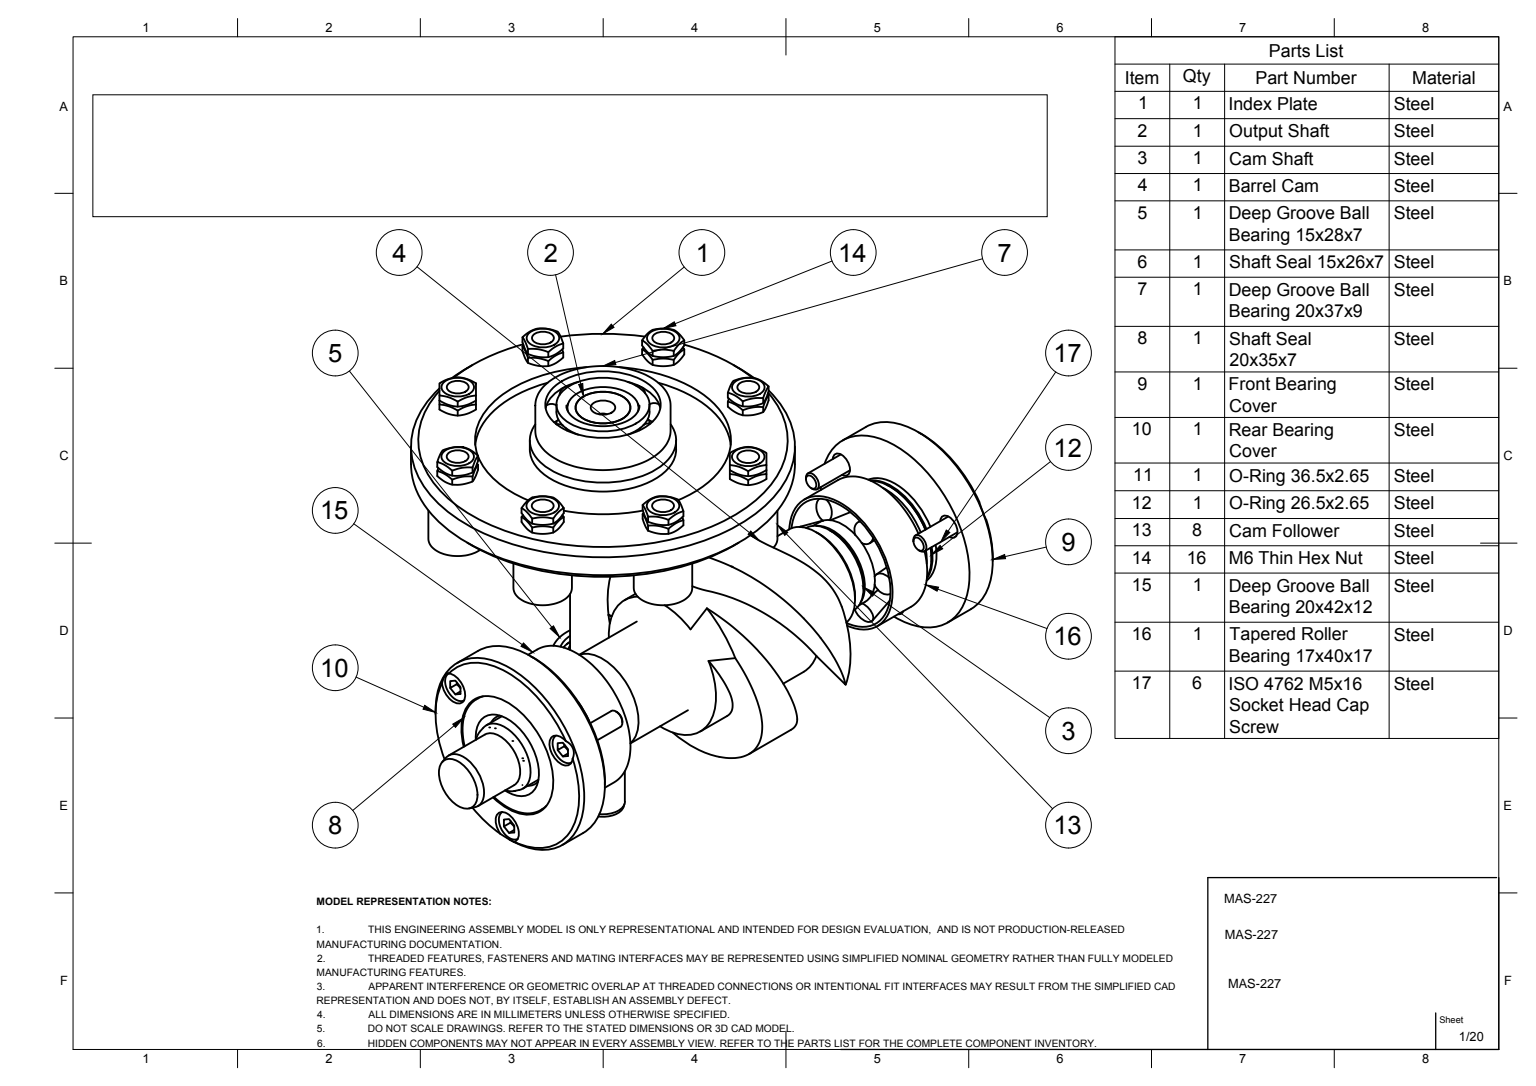
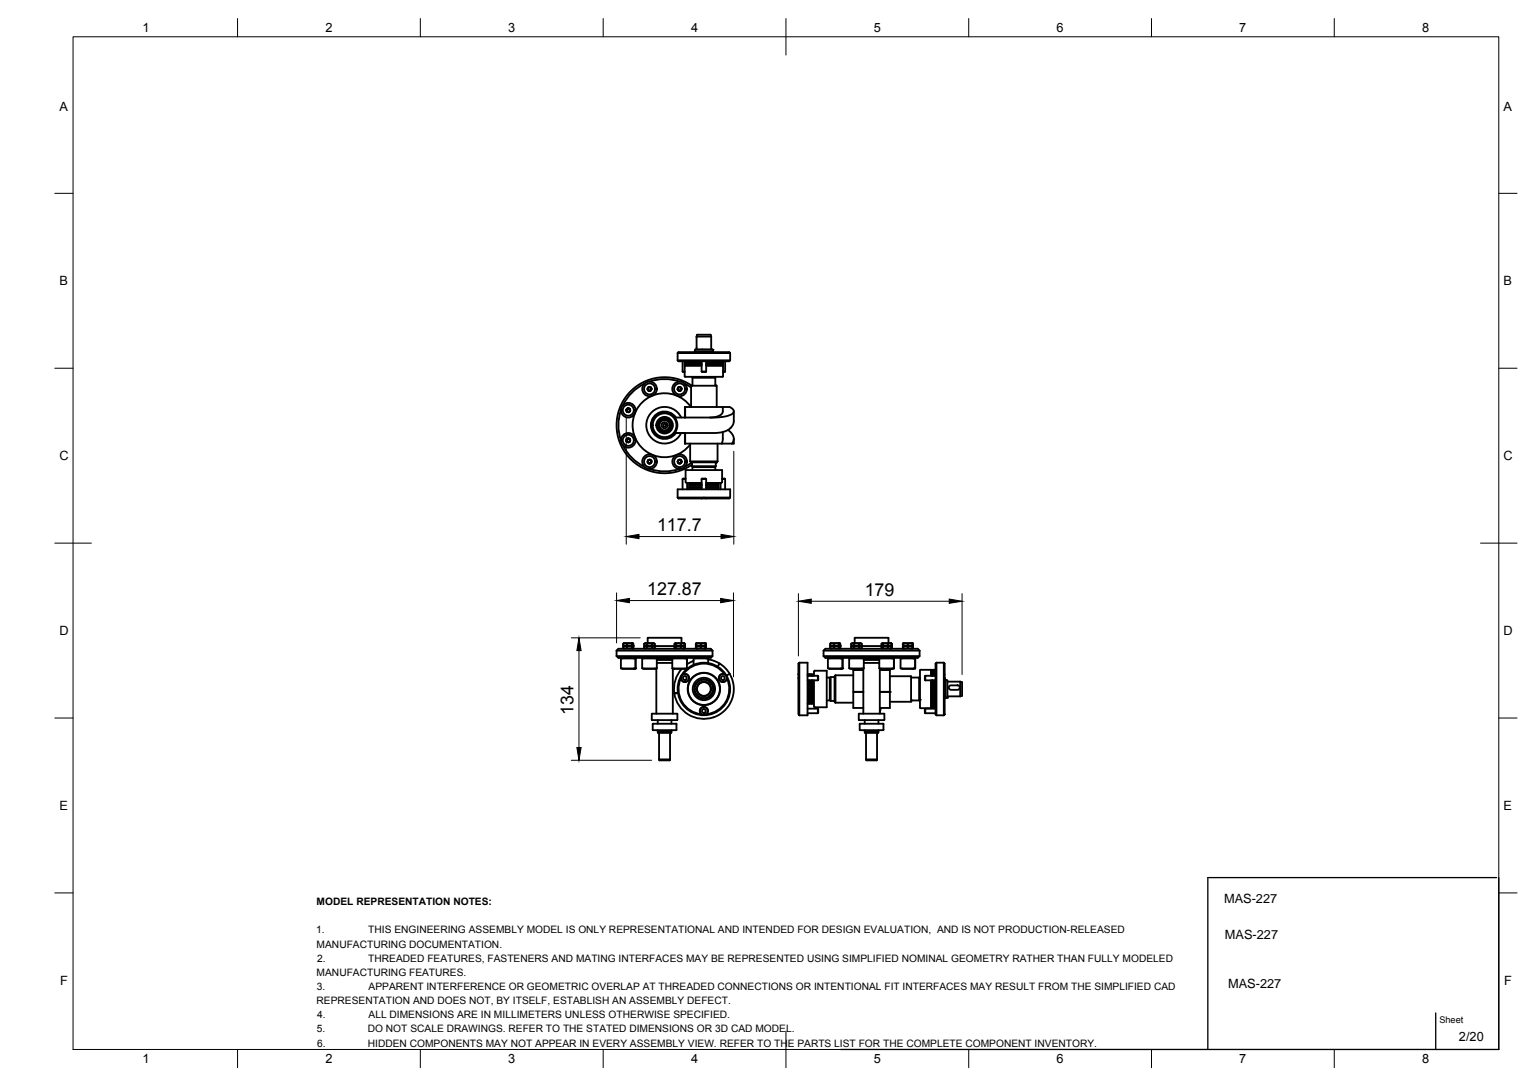
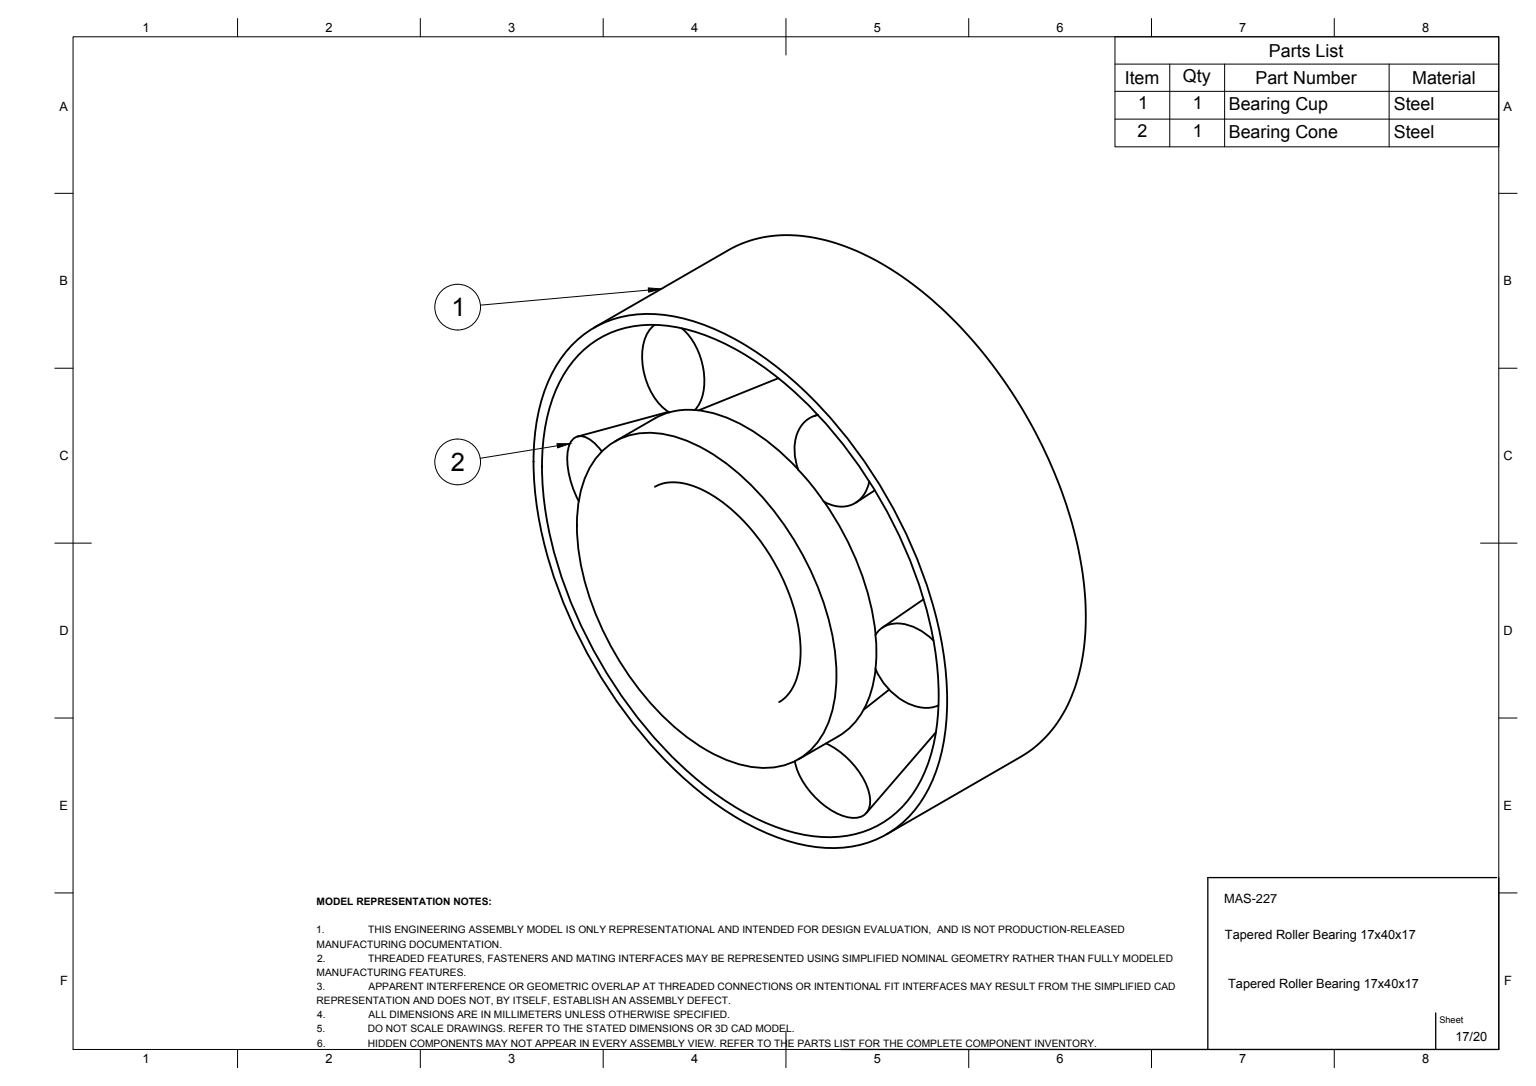
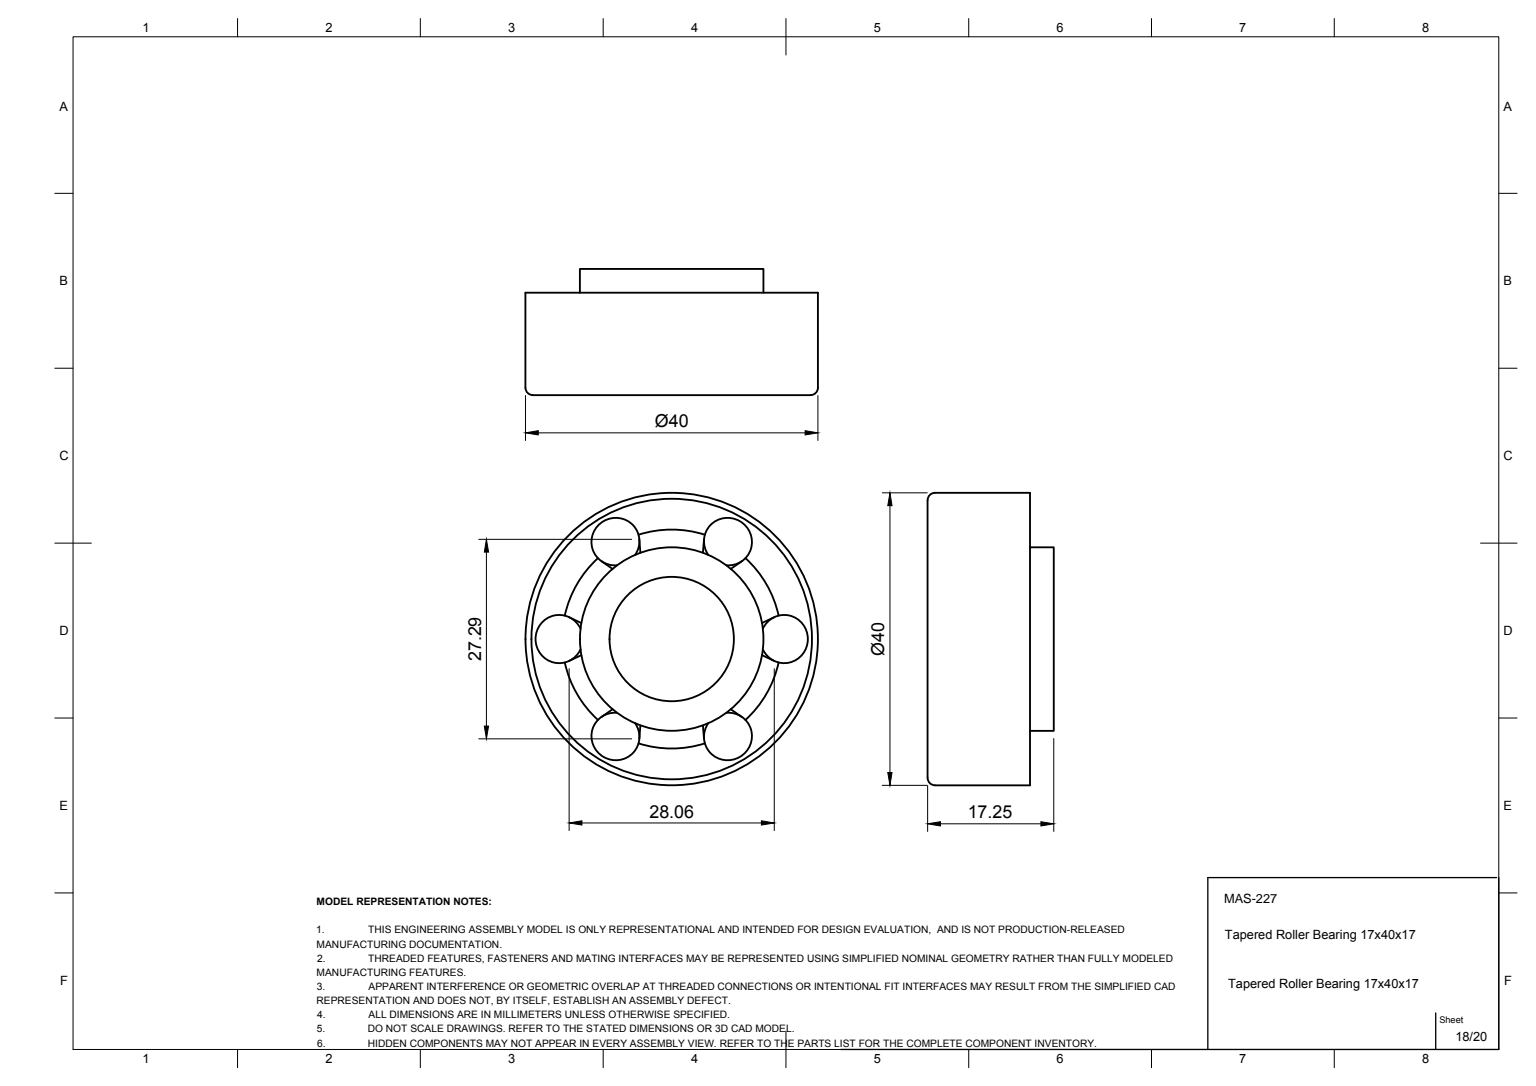
ISO-10303-21;
HEADER;
FILE_DESCRIPTION (('STEP AP214'),
    '1' );
FILE_NAME ( 'MAS-227', '2026-10-06T08:24:41', ( '' ), ( '' ), 'STEP AP214', 'Unspecified', '' );
FILE_SCHEMA (( 'AUTOMOTIVE_DESIGN' ));
ENDSEC;
DATA;
#1 = ORIENTED_EDGE ( 'NONE', *, *, #7056, .T. ) ;
#2 = LINE ( 'NONE', #16920, #12528 ) ;
#3 = CARTESIAN_POINT ( 'NONE',  ( -0.4535326485287288212, 0.08054850140359781641, 0.1903859677775356918 ) ) ;
#4 = EDGE_LOOP ( 'NONE', ( #17805, #23711 ) ) ;
#5 = EDGE_CURVE ( 'NONE', #3462, #12596, #11883, .T. ) ;
#6 = CARTESIAN_POINT ( 'NONE',  ( 0.3607825703614780388, 0.06309631803704385256, 0.08455817587619855746 ) ) ;
#7 = DIRECTION ( 'NONE',  ( -1.000000000000000000, 0.000000000000000000, 0.000000000000000000 ) ) ;
#8 = CARTESIAN_POINT ( 'NONE',  ( 0.4441657790107835790, 0.2564944395515610931, 1.766732283464566899 ) ) ;
#9 = CARTESIAN_POINT ( 'NONE',  ( -0.4441657790107816917, 0.2564944395515652564, 1.747047244094488194 ) ) ;
#10 = DIRECTION ( 'NONE',  ( 0.000000000000000000, 0.000000000000000000, -1.000000000000000000 ) ) ;
#11 = ORIENTED_EDGE ( 'NONE', *, *, #14941, .F. ) ;
#12 = ORIENTED_EDGE ( 'NONE', *, *, #1724, .F. ) ;
#13 = AXIS2_PLACEMENT_3D ( 'NONE', #19056, #4369, #12570 ) ;
#14 = CARTESIAN_POINT ( 'NONE',  ( 0.3392387706403788838, 0.1151913129404419922, -3.115157480314960647 ) ) ;
#15 = EDGE_LOOP ( 'NONE', ( #27467, #1263, #14618, #2315 ) ) ;
#16 = VECTOR ( 'NONE', #25665, 39.37007874015748143 ) ;
#17 = EDGE_LOOP ( 'NONE', ( #23357, #276 ) ) ;
#18 = FACE_OUTER_BOUND ( 'NONE', #11254, .T. ) ;
#19 = ( CONVERSION_BASED_UNIT ( 'INCH', #19315 ) LENGTH_UNIT ( ) NAMED_UNIT ( #4330 ) ) ;
#20 = CARTESIAN_POINT ( 'NONE',  ( 0.3339160553493882300, 0.9180073733179625606, -0.7185233507685039323 ) ) ;
#21 = CARTESIAN_POINT ( 'NONE',  ( 0.3324885138898234782, -0.04380447413659139394, 1.973425196850393970 ) ) ;
#22 = ORIENTED_EDGE ( 'NONE', *, *, #12287, .T. ) ;
#23 = EDGE_CURVE ( 'NONE', #19722, #14586, #4579, .T. ) ;
#24 = ORIENTED_EDGE ( 'NONE', *, *, #27873, .F. ) ;
#25 = VERTEX_POINT ( 'NONE', #21962 ) ;
#26 = AXIS2_PLACEMENT_3D ( 'NONE', #24045, #13033, #11185 ) ;
#27 = ORIENTED_EDGE ( 'NONE', *, *, #23684, .F. ) ;
#28 = EDGE_LOOP ( 'NONE', ( #27536, #25941, #6890, #26998 ) ) ;
#29 = ORIENTED_EDGE ( 'NONE', *, *, #17755, .F. ) ;
#30 = CARTESIAN_POINT ( 'NONE',  ( -0.5949363243629232079, -0.1357903337134990229, 0.2362204724409449064 ) ) ;
#31 = ( BOUNDED_CURVE ( )  B_SPLINE_CURVE ( 2, ( #4927, #4785, #24416 ),
 .UNSPECIFIED., .F., .T. ) 
 B_SPLINE_CURVE_WITH_KNOTS ( ( 3, 3 ),
 ( 0.000000000000000000, 0.5842180690389588982 ),
 .UNSPECIFIED. ) 
 CURVE ( )  GEOMETRIC_REPRESENTATION_ITEM ( )  RATIONAL_B_SPLINE_CURVE ( ( 1.000000000000000000, 1.154700538379253905, 1.000000000000000000 ) ) 
 REPRESENTATION_ITEM ( '' )  ) ;
#32 = ITEM_DEFINED_TRANSFORMATION ( 'NONE', 'NONE', #4428,  #11588 ) ;
#33 = EDGE_CURVE ( 'NONE', #1582, #19320, #13242, .T. ) ;
#34 = CARTESIAN_POINT ( 'NONE',  ( 0.3976891862754212137, 0.7181140751201200434, -0.6642661073933326943 ) ) ;
#35 = LINE ( 'NONE', #6897, #10289 ) ;
#36 = CARTESIAN_POINT ( 'NONE',  ( 0.4620608682196346573, 0.08206165078060492779, 0.1992125984251968684 ) ) ;
#37 = ORIENTED_EDGE ( 'NONE', *, *, #10875, .F. ) ;
#38 = AXIS2_PLACEMENT_3D ( 'NONE', #5001, #26071, #6729 ) ;
#39 = CARTESIAN_POINT ( 'NONE',  ( 0.000000000000000000, 0.000000000000000000, 0.06614173228346456601 ) ) ;
#40 = CARTESIAN_POINT ( 'NONE',  ( -2.184900367198595585E-17, 0.6212598425196850238, 0.2574827755769818483 ) ) ;
#41 = DIRECTION ( 'NONE',  ( 0.000000000000000000, 0.000000000000000000, -1.000000000000000000 ) ) ;
#42 = CARTESIAN_POINT ( 'NONE',  ( -0.3649820351482981340, -1.095990260593795451, -0.3743461065083169559 ) ) ;
#43 = CARTESIAN_POINT ( 'NONE',  ( 0.000000000000000000, 0.000000000000000000, 0.2362204724409449064 ) ) ;
#44 = DIRECTION ( 'NONE',  ( -0.000000000000000000, -1.000000000000000000, -0.000000000000000000 ) ) ;
#45 = EDGE_CURVE ( 'NONE', #18347, #8484, #23181, .T. ) ;
#46 = CARTESIAN_POINT ( 'NONE',  ( -0.08600259748440698682, 0.2165354330708661457, -3.223068998490977499 ) ) ;
#47 = ORIENTED_EDGE ( 'NONE', *, *, #24932, .T. ) ;
#48 = ORIENTED_EDGE ( 'NONE', *, *, #8188, .T. ) ;
#49 = DIRECTION ( 'NONE',  ( 0.000000000000000000, 0.000000000000000000, 1.000000000000000000 ) ) ;
#50 = AXIS2_PLACEMENT_3D ( 'NONE', #26604, #25051, #22376 ) ;
#51 = VERTEX_POINT ( 'NONE', #494 ) ;
#52 = VECTOR ( 'NONE', #14977, 39.37007874015748143 ) ;
#53 = DIRECTION ( 'NONE',  ( 0.000000000000000000, 0.000000000000000000, 1.000000000000000000 ) ) ;
#54 = DIRECTION ( 'NONE',  ( 1.000000000000000000, 0.000000000000000000, 0.000000000000000000 ) ) ;
#55 = EDGE_CURVE ( 'NONE', #27011, #13237, #9086, .T. ) ;
#56 = CARTESIAN_POINT ( 'NONE',  ( -0.5476281405333500718, 0.07214854559197644845, 0.9399606299212598381 ) ) ;
#57 = EDGE_CURVE ( 'NONE', #14897, #14790, #10537, .T. ) ;
#58 = CARTESIAN_POINT ( 'NONE',  ( 0.4771018889076559244, 0.3804760601893846794, 0.2362204724409449064 ) ) ;
#59 = ORIENTED_EDGE ( 'NONE', *, *, #13176, .F. ) ;
#60 = CARTESIAN_POINT ( 'NONE',  ( -0.4335958738490826581, -0.2505647196907692664, 0.09684793308443542803 ) ) ;
#61 = AXIS2_PLACEMENT_3D ( 'NONE', #22056, #14008, #15706 ) ;
#62 = CARTESIAN_POINT ( 'NONE',  ( 0.2428345617565153547, 0.2885915454824177218, 0.1992125984251968684 ) ) ;
#63 = ADVANCED_FACE ( 'NONE', ( #7520 ), #26320, .F. ) ;
#64 = CARTESIAN_POINT ( 'NONE',  ( 0.4157391792961063204, 0.3323952789219082882, 0.1322834645669291320 ) ) ;
#65 = CARTESIAN_POINT ( 'NONE',  ( 0.000000000000000000, 0.000000000000000000, -0.2618110236220472231 ) ) ;
#66 = DIRECTION ( 'NONE',  ( 0.000000000000000000, 0.000000000000000000, 1.000000000000000000 ) ) ;
#67 = CARTESIAN_POINT ( 'NONE',  ( 0.8031496062992127261, 0.000000000000000000, 0.4488188976377953110 ) ) ;
#68 = CARTESIAN_POINT ( 'NONE',  ( 0.1516263115863346334, -0.2937912646890007973, 0.3972688187320929099 ) ) ;
#69 = DIRECTION ( 'NONE',  ( 1.000000000000000000, 0.000000000000000000, 0.000000000000000000 ) ) ;
#70 = FACE_OUTER_BOUND ( 'NONE', #14571, .T. ) ;
#71 = DIRECTION ( 'NONE',  ( 0.000000000000000000, 0.000000000000000000, 1.000000000000000000 ) ) ;
#72 = CARTESIAN_POINT ( 'NONE',  ( 0.3339160553493882300, 0.7867001919223544082, -0.8344257386302499357 ) ) ;
#73 = AXIS2_PLACEMENT_3D ( 'NONE', #23725, #21593, #23590 ) ;
#74 = CARTESIAN_POINT ( 'NONE',  ( 0.1480156394741928561, -0.5526079293736928522, 0.9399606299212598381 ) ) ;
#75 = DIRECTION ( 'NONE',  ( -1.000000000000000000, 0.000000000000000000, 0.000000000000000000 ) ) ;
#76 = ORIENTED_EDGE ( 'NONE', *, *, #16694, .F. ) ;
#77 = CARTESIAN_POINT ( 'NONE',  ( 0.04673558830902516809, 0.3552036222399216903, -3.115157480314960647 ) ) ;
#78 = VECTOR ( 'NONE', #27167, 39.37007874015748854 ) ;
#79 = EDGE_LOOP ( 'NONE', ( #24549, #12991, #16155, #19629, #1630 ) ) ;
#80 = EDGE_LOOP ( 'NONE', ( #10881, #7158 ) ) ;
#81 = EDGE_CURVE ( 'NONE', #10766, #14002, #19559, .T. ) ;
#82 = CARTESIAN_POINT ( 'NONE',  ( 0.4856708409191422549, -0.1649135259639211148, -1.550196850393700920 ) ) ;
#83 = DIRECTION ( 'NONE',  ( 0.000000000000000000, 0.000000000000000000, 1.000000000000000000 ) ) ;
#84 = CARTESIAN_POINT ( 'NONE',  ( 0.5144793533649091311, -0.1379038425970198489, 1.747047244094488416 ) ) ;
#85 = ORIENTED_EDGE ( 'NONE', *, *, #20703, .F. ) ;
#86 = EDGE_CURVE ( 'NONE', #9806, #21006, #24069, .T. ) ;
#87 = FACE_BOUND ( 'NONE', #23508, .T. ) ;
#88 = VERTEX_POINT ( 'NONE', #13082 ) ;
#89 = DIRECTION ( 'NONE',  ( 0.000000000000000000, -1.000000000000000000, 0.000000000000000000 ) ) ;
#90 = CIRCLE ( 'NONE', #23529, 0.3937007874015748254 ) ;
#91 = CYLINDRICAL_SURFACE ( 'NONE', #13414, 0.4941010236220472751 ) ;
#92 = DIRECTION ( 'NONE',  ( -0.8660254037844387076, 0.4999999999999998890, 0.000000000000000000 ) ) ;
#93 = SURFACE_STYLE_USAGE ( .BOTH. , #2166 ) ;
#94 = DIRECTION ( 'NONE',  ( -1.000000000000000000, 0.000000000000000000, 0.000000000000000000 ) ) ;
#95 = CARTESIAN_POINT ( 'NONE',  ( 0.1709077104829875848, -0.4707213777573787672, 0.09684874903502814492 ) ) ;
#96 = ORIENTED_EDGE ( 'NONE', *, *, #21914, .F. ) ;
#97 = LINE ( 'NONE', #15591, #22935 ) ;
#98 = CARTESIAN_POINT ( 'NONE',  ( -0.4055118110236220486, 4.966087413865251393E-17, 0.3543307086614173040 ) ) ;
#99 = CARTESIAN_POINT ( 'NONE',  ( -0.3001918266901933974, 0.3912931228432126596, -1.550196850393700920 ) ) ;
#100 = PRODUCT_DEFINITION_CONTEXT ( 'detailed design', #9805, 'design' ) ;
#101 = CARTESIAN_POINT ( 'NONE',  ( 0.1458850421962362143, -0.4296318976989931815, -1.934055118110236338 ) ) ;
#102 = DIRECTION ( 'NONE',  ( -1.000000000000000000, 0.000000000000000000, 0.000000000000000000 ) ) ;
#103 = CARTESIAN_POINT ( 'NONE',  ( 0.1669771619554775988, -0.4570419016558947556, 0.1827409795206137999 ) ) ;
#104 = CARTESIAN_POINT ( 'NONE',  ( -0.6505662911506299162, -0.01797296504513622162, 0.07864818162991654704 ) ) ;
#105 = FILL_AREA_STYLE_COLOUR ( '', #1895 ) ;
#106 = DIRECTION ( 'NONE',  ( -1.000000000000000000, 0.000000000000000000, -0.000000000000000000 ) ) ;
#107 = ORIENTED_EDGE ( 'NONE', *, *, #20255, .T. ) ;
#108 = EDGE_LOOP ( 'NONE', ( #16831, #22102, #23011, #14973, #23434 ) ) ;
#109 = ADVANCED_FACE ( 'NONE', ( #134 ), #14626, .F. ) ;
#110 = CIRCLE ( 'NONE', #17215, 0.4848217985909654137 ) ;
#111 = FACE_OUTER_BOUND ( 'NONE', #23572, .T. ) ;
#112 = AXIS2_PLACEMENT_3D ( 'NONE', #26701, #7362, #3107 ) ;
#113 = CARTESIAN_POINT ( 'NONE',  ( -0.3350125228558759050, 0.2937477835494528011, -1.934055118110236560 ) ) ;
#114 = EDGE_CURVE ( 'NONE', #14474, #3555, #20012, .T. ) ;
#115 = CARTESIAN_POINT ( 'NONE',  ( -0.7432982829791772161, 0.2032415433700952845, -0.2614846436432287091 ) ) ;
#116 = EDGE_LOOP ( 'NONE', ( #3270, #475, #22588, #2347 ) ) ;
#117 = DIRECTION ( 'NONE',  ( -1.000000000000000000, 0.000000000000000000, 0.000000000000000000 ) ) ;
#118 = CARTESIAN_POINT ( 'NONE',  ( -0.1839420097223181394, -0.5417097841048805762, 0.9399606299212598381 ) ) ;
#119 = CARTESIAN_POINT ( 'NONE',  ( 0.3334645669291338987, -0.9593003268715946108, -0.8847456892490688229 ) ) ;
#120 = ( REPRESENTATION_RELATIONSHIP ('NONE','NONE', #12434, #25798 ) REPRESENTATION_RELATIONSHIP_WITH_TRANSFORMATION ( #8739 )SHAPE_REPRESENTATION_RELATIONSHIP( ) ) ;
#121 = DIRECTION ( 'NONE',  ( 0.000000000000000000, -0.8660254037844385966, 0.4999999999999998335 ) ) ;
#122 = AXIS2_PLACEMENT_3D ( 'NONE', #22797, #14633, #3420 ) ;
#123 = CARTESIAN_POINT ( 'NONE',  ( 0.3858827008519146728, -0.2227458012931471110, -1.934055118110236338 ) ) ;
#124 = CARTESIAN_POINT ( 'NONE',  ( 0.3233561589689052385, -0.1867299569291582528, -3.115157480314960647 ) ) ;
#125 = DIRECTION ( 'NONE',  ( 0.000000000000000000, -1.000000000000000000, 0.000000000000000000 ) ) ;
#126 = CARTESIAN_POINT ( 'NONE',  ( 0.0005789221761808661720, 0.4692909815006409691, 0.1992125984251968684 ) ) ;
#127 = DIRECTION ( 'NONE',  ( -1.000000000000000000, 0.000000000000000000, 0.000000000000000000 ) ) ;
#128 = CARTESIAN_POINT ( 'NONE',  ( 0.000000000000000000, 0.000000000000000000, 0.01181102362204724393 ) ) ;
#129 = EDGE_CURVE ( 'NONE', #7282, #11900, #2406, .T. ) ;
#130 = TOROIDAL_SURFACE ( 'NONE', #25799, 0.5610236220472440971, 0.1003937007874015908 ) ;
#131 = DIRECTION ( 'NONE',  ( 0.000000000000000000, 0.000000000000000000, -1.000000000000000000 ) ) ;
#132 = CIRCLE ( 'NONE', #21747, 0.6299212598425196763 ) ;
#133 = ORIENTED_EDGE ( 'NONE', *, *, #949, .F. ) ;
#134 = FACE_OUTER_BOUND ( 'NONE', #7605, .T. ) ;
#135 = ORIENTED_EDGE ( 'NONE', *, *, #15589, .F. ) ;
#136 = CARTESIAN_POINT ( 'NONE',  ( 0.000000000000000000, 0.000000000000000000, 0.2362204724409449064 ) ) ;
#137 = DIRECTION ( 'NONE',  ( 0.000000000000000000, 0.000000000000000000, 1.000000000000000000 ) ) ;
#138 = CARTESIAN_POINT ( 'NONE',  ( -0.4069448477556107946, -0.3121994997598286914, 1.766732283464566899 ) ) ;
#139 = DIRECTION ( 'NONE',  ( 0.000000000000000000, 0.000000000000000000, 1.000000000000000000 ) ) ;
#140 = ORIENTED_EDGE ( 'NONE', *, *, #5854, .T. ) ;
#141 = TOROIDAL_SURFACE ( 'NONE', #14548, 0.5915354330708662012, 0.05216535433070866590 ) ;
#142 = ORIENTED_EDGE ( 'NONE', *, *, #15280, .T. ) ;
#144 = CARTESIAN_POINT ( 'NONE',  ( 0.3460635936745020680, -0.09269288654273737105, -3.115157480314960647 ) ) ;
#143 = CARTESIAN_POINT ( 'NONE',  ( 0.5614173959481695286, 0.4467232815848914962, 0.1601585119481469810 ) ) ;
#145 = ORIENTED_EDGE ( 'NONE', *, *, #17289, .F. ) ;
#146 = CARTESIAN_POINT ( 'NONE',  ( -2.183966630091013010E-17, 0.6212598425196852459, 0.09684793308443542803 ) ) ;
#147 = VERTEX_POINT ( 'NONE', #612 ) ;
#148 = CARTESIAN_POINT ( 'NONE',  ( 0.07874015748031495954, -0.04546065111729338803, -0.4724409448818898127 ) ) ;
#149 = DIRECTION ( 'NONE',  ( 1.000000000000000000, 0.000000000000000000, 0.000000000000000000 ) ) ;
#150 = ADVANCED_FACE ( 'NONE', ( #5405 ), #14023, .T. ) ;
#151 = ORIENTED_EDGE ( 'NONE', *, *, #4349, .F. ) ;
#152 = VERTEX_POINT ( 'NONE', #7235 ) ;
#153 = AXIS2_PLACEMENT_3D ( 'NONE', #12101, #3470, #22847 ) ;
#154 = ADVANCED_FACE ( 'NONE', ( #2979 ), #26440, .T. ) ;
#155 = CARTESIAN_POINT ( 'NONE',  ( 0.000000000000000000, 0.000000000000000000, 0.9055118110027171596 ) ) ;
#156 = ORIENTED_EDGE ( 'NONE', *, *, #27125, .T. ) ;
#157 = ORIENTED_EDGE ( 'NONE', *, *, #9364, .T. ) ;
#158 = VERTEX_POINT ( 'NONE', #15724 ) ;
#159 = CARTESIAN_POINT ( 'NONE',  ( -0.1771653543307086520, -5.663984251968503442E-18, 0.000000000000000000 ) ) ;
#160 = DIRECTION ( 'NONE',  ( 0.000000000000000000, 0.000000000000000000, 1.000000000000000000 ) ) ;
#161 = CARTESIAN_POINT ( 'NONE',  ( 0.000000000000000000, 0.000000000000000000, -0.1033464566929133965 ) ) ;
#162 = CARTESIAN_POINT ( 'NONE',  ( 0.09842519685039370636, 0.2165354330708661457, -3.456364829396325167 ) ) ;
#163 = PRODUCT ( 'M6 Thin Hex Nut', 'M6 Thin Hex Nut', '', ( #11511 ) ) ;
#164 = CIRCLE ( 'NONE', #26696, 1.988188976448617584 ) ;
#165 = CARTESIAN_POINT ( 'NONE',  ( 0.000000000000000000, 0.000000000000000000, -3.278217716535432842E-17 ) ) ;
#166 = CARTESIAN_POINT ( 'NONE',  ( 0.1490609433494345659, -0.2352065284464384953, -0.4168512521180542385 ) ) ;
#167 = DIRECTION ( 'NONE',  ( 1.000000000000000000, 0.000000000000000000, 0.000000000000000000 ) ) ;
#168 = CARTESIAN_POINT ( 'NONE',  ( -0.2120693917185543231, -0.5839438448129543602, 0.09684874924366436433 ) ) ;
#169 = EDGE_CURVE ( 'NONE', #21708, #16172, #21378, .T. ) ;
#170 = CIRCLE ( 'NONE', #27197, 0.2952755905264887182 ) ;
#171 = CARTESIAN_POINT ( 'NONE',  ( -0.3799403784234969272, -1.031940123604548010, -0.2795979895621366063 ) ) ;
#172 = CARTESIAN_POINT ( 'NONE',  ( -0.6029881478123397809, 1.118968434182175953, 0.03326447829408156476 ) ) ;
#173 = FACE_OUTER_BOUND ( 'NONE', #11804, .T. ) ;
#174 = CARTESIAN_POINT ( 'NONE',  ( -0.07870736599817811097, 0.1968503937007873850, -3.212150913008701814 ) ) ;
#175 = EDGE_LOOP ( 'NONE', ( #22367, #5338, #24383, #19393 ) ) ;
#176 = ADVANCED_FACE ( 'NONE', ( #13590 ), #15218, .F. ) ;
#177 = DIRECTION ( 'NONE',  ( 0.000000000000000000, 0.000000000000000000, 1.000000000000000000 ) ) ;
#178 = CARTESIAN_POINT ( 'NONE',  ( 0.000000000000000000, 0.000000000000000000, 0.2362204724409449064 ) ) ;
#179 = VECTOR ( 'NONE', #19878, 39.37007874015748143 ) ;
#180 = ORIENTED_EDGE ( 'NONE', *, *, #22193, .F. ) ;
#181 = ( BOUNDED_CURVE ( )  B_SPLINE_CURVE ( 3, ( #15130, #19634, #17231, #21476 ),
 .UNSPECIFIED., .F., .F. ) 
 B_SPLINE_CURVE_WITH_KNOTS ( ( 4, 4 ),
 ( 6.170019055269735375, 6.396351559089437089 ),
 .UNSPECIFIED. ) 
 CURVE ( )  GEOMETRIC_REPRESENTATION_ITEM ( )  RATIONAL_B_SPLINE_CURVE ( ( 1.000000000000000000, 0.9957356870045847019, 0.9957356870045847019, 1.000000000000000000 ) ) 
 REPRESENTATION_ITEM ( '' )  ) ;
#182 = CIRCLE ( 'NONE', #19069, 0.2952755905511810774 ) ;
#183 = CARTESIAN_POINT ( 'NONE',  ( 0.1259842519685039353, 0.1751968503937007815, 0.000000000000000000 ) ) ;
#184 = CARTESIAN_POINT ( 'NONE',  ( 0.4932478747986535628, 0.08657132889677619791, 0.09684874903502814492 ) ) ;
#185 = CARTESIAN_POINT ( 'NONE',  ( 0.0007595033562148819414, 0.6881885572739390167, 0.1322834645669291320 ) ) ;
#186 = B_SPLINE_CURVE_WITH_KNOTS ( 'NONE', 3,
 ( #3405, #6229, #8475, #4376, #23337, #25576 ),
 .UNSPECIFIED., .F., .F.,
 ( 4, 2, 4 ),
 ( 0.2291966065698869959, 0.2305109203526899964, 0.2318252341354939960 ),
 .UNSPECIFIED. ) ;
#187 = ORIENTED_EDGE ( 'NONE', *, *, #16548, .F. ) ;
#188 = CARTESIAN_POINT ( 'NONE',  ( -0.4382482975805212511, 0.3362148458989001609, 0.9399606299212598381 ) ) ;
#189 = ORIENTED_EDGE ( 'NONE', *, *, #329, .F. ) ;
#190 = CARTESIAN_POINT ( 'NONE',  ( -0.6299212598425196763, -0.4724409448818898127, -0.8182917201112815953 ) ) ;
#191 = ORIENTED_EDGE ( 'NONE', *, *, #12482, .T. ) ;
#192 = DIRECTION ( 'NONE',  ( -1.000000000000000000, 0.000000000000000000, 0.000000000000000000 ) ) ;
#193 = CIRCLE ( 'NONE', #14146, 0.1181102362204720091 ) ;
#194 = CARTESIAN_POINT ( 'NONE',  ( 0.000000000000000000, 0.000000000000000000, -0.2204724409448818867 ) ) ;
#195 = CARTESIAN_POINT ( 'NONE',  ( 0.000000000000000000, 0.000000000000000000, -3.278217716535432842E-17 ) ) ;
#196 = CARTESIAN_POINT ( 'NONE',  ( -0.6751968503937006982, 0.000000000000000000, -0.2618110236220472231 ) ) ;
#197 = CARTESIAN_POINT ( 'NONE',  ( -0.3149606299212598381, 0.000000000000000000, -0.03543307086614204404 ) ) ;
#198 = CARTESIAN_POINT ( 'NONE',  ( -0.1709077104829878069, -0.4707213777573787672, 0.09684874903502814492 ) ) ;
#199 = CARTESIAN_POINT ( 'NONE',  ( -0.3665264996331779601, -0.2116141732283464416, 0.1377952755905511861 ) ) ;
#200 = DIRECTION ( 'NONE',  ( 0.000000000000000000, -1.000000000000000000, 0.000000000000000000 ) ) ;
#201 = DIRECTION ( 'NONE',  ( -0.000000000000000000, -1.000000000000000000, -0.000000000000000000 ) ) ;
#202 = DIRECTION ( 'NONE',  ( 0.000000000000000000, 0.000000000000000000, 1.000000000000000000 ) ) ;
#203 = ADVANCED_FACE ( 'NONE', ( #17324 ), #15936, .F. ) ;
#204 = CIRCLE ( 'NONE', #17722, 0.6212598425196850238 ) ;
#205 = CARTESIAN_POINT ( 'NONE',  ( 0.07472527936312040042, -0.5671862884095228985, 0.9399606299212598381 ) ) ;
#206 = DIRECTION ( 'NONE',  ( 0.000000000000000000, 1.000000000000000000, 0.000000000000000000 ) ) ;
#207 = ORIENTED_EDGE ( 'NONE', *, *, #6942, .F. ) ;
#208 = CARTESIAN_POINT ( 'NONE',  ( -0.01968503937007897581, -0.8214970631411201429, 0.000000000000000000 ) ) ;
#209 = EDGE_CURVE ( 'NONE', #16657, #13154, #17294, .T. ) ;
#210 = CIRCLE ( 'NONE', #27230, 0.6212598425196850238 ) ;
#211 = EDGE_CURVE ( 'NONE', #8069, #8578, #17150, .T. ) ;
#212 = AXIS2_PLACEMENT_3D ( 'NONE', #21327, #27824, #8463 ) ;
#213 = ORIENTED_EDGE ( 'NONE', *, *, #16639, .F. ) ;
#214 = VERTEX_POINT ( 'NONE', #20374 ) ;
#215 = CARTESIAN_POINT ( 'NONE',  ( 0.4954757973265890847, -0.2860025288253325582, 0.9399606299212601712 ) ) ;
#216 = LINE ( 'NONE', #2154, #15629 ) ;
#217 = CARTESIAN_POINT ( 'NONE',  ( -1.928513779527558736E-17, 0.000000000000000000, -0.4566929133858267376 ) ) ;
#218 = VERTEX_POINT ( 'NONE', #1034 ) ;
#219 = VECTOR ( 'NONE', #3397, 39.37007874015748143 ) ;
#220 = CARTESIAN_POINT ( 'NONE',  ( 0.000000000000000000, 0.000000000000000000, 0.1771653543307086520 ) ) ;
#221 = EDGE_LOOP ( 'NONE', ( #12338, #6881, #25054, #27642 ) ) ;
#222 = SURFACE_STYLE_USAGE ( .BOTH. , #19537 ) ;
#223 = CARTESIAN_POINT ( 'NONE',  ( 0.0005057506112066243896, 0.6881888373222778688, 0.3401591245381555551 ) ) ;
#224 = ( CONVERSION_BASED_UNIT ( 'INCH', #8931 ) LENGTH_UNIT ( ) NAMED_UNIT ( #18982 ) ) ;
#225 = CIRCLE ( 'NONE', #16892, 0.5007874015748031704 ) ;
#226 = CARTESIAN_POINT ( 'NONE',  ( 0.0005189969344232283309, 0.3771649972486724733, 0.07637795275590551769 ) ) ;
#227 = AXIS2_PLACEMENT_3D ( 'NONE', #3508, #14722, #27552 ) ;
#228 = ORIENTED_EDGE ( 'NONE', *, *, #21922, .T. ) ;
#229 = CARTESIAN_POINT ( 'NONE',  ( 0.03008364706454716778, 0.1136516277932332619, 0.1968503937007874127 ) ) ;
#230 = ADVANCED_FACE ( 'NONE', ( #18229 ), #8731, .T. ) ;
#231 = DIRECTION ( 'NONE',  ( 0.000000000000000000, 0.000000000000000000, 1.000000000000000000 ) ) ;
#232 = EDGE_CURVE ( 'NONE', #4548, #1758, #3760, .T. ) ;
#233 = EDGE_CURVE ( 'NONE', #14152, #23049, #22735, .T. ) ;
#234 = AXIS2_PLACEMENT_3D ( 'NONE', #13814, #26508, #13665 ) ;
#235 = EDGE_CURVE ( 'NONE', #27620, #935, #8316, .T. ) ;
#236 = CARTESIAN_POINT ( 'NONE',  ( -0.6370261810203012853, -0.04389326872400071272, -0.2373533611760622331 ) ) ;
#237 = FACE_OUTER_BOUND ( 'NONE', #646, .T. ) ;
#238 = SURFACE_STYLE_USAGE ( .BOTH. , #19827 ) ;
#239 = EDGE_LOOP ( 'NONE', ( #22677, #15160 ) ) ;
#240 = VERTEX_POINT ( 'NONE', #18659 ) ;
#241 = EDGE_CURVE ( 'NONE', #21409, #11103, #22772, .T. ) ;
#242 = AXIS2_PLACEMENT_3D ( 'NONE', #867, #7637, #22743 ) ;
#243 = FACE_OUTER_BOUND ( 'NONE', #27157, .T. ) ;
#244 = CIRCLE ( 'NONE', #20043, 0.1751968503937007815 ) ;
#245 = DIRECTION ( 'NONE',  ( -1.000000000000000000, 0.000000000000000000, 0.000000000000000000 ) ) ;
#246 = CARTESIAN_POINT ( 'NONE',  ( 0.1490609433615242285, 0.4786070381542913421, 0.000000000000000000 ) ) ;
#247 = VERTEX_POINT ( 'NONE', #23212 ) ;
#248 = CARTESIAN_POINT ( 'NONE',  ( 0.3998447049182889956, 0.4754871227240441423, 0.2574803149606298969 ) ) ;
#249 = ORIENTED_EDGE ( 'NONE', *, *, #1427, .F. ) ;
#250 = CARTESIAN_POINT ( 'NONE',  ( -0.7795729917428700917, 0.3988254141273629982, 0.006455232907575630084 ) ) ;
#251 = EDGE_CURVE ( 'NONE', #10904, #1560, #4337, .T. ) ;
#252 = ORIENTED_EDGE ( 'NONE', *, *, #21026, .F. ) ;
#253 = DIRECTION ( 'NONE',  ( -1.000000000000000000, 0.000000000000000000, 0.000000000000000000 ) ) ;
#254 = CARTESIAN_POINT ( 'NONE',  ( 0.3722026523000413478, 4.558167867734008572E-17, -0.07578740157480315376 ) ) ;
#255 = CARTESIAN_POINT ( 'NONE',  ( -0.03736310157557653361, -0.5708661417322835607, 0.9399606299212598381 ) ) ;
#256 = DIRECTION ( 'NONE',  ( 0.000000000000000000, 0.000000000000000000, 1.000000000000000000 ) ) ;
#257 = AXIS2_PLACEMENT_3D ( 'NONE', #24962, #7448, #3195 ) ;
#258 = CARTESIAN_POINT ( 'NONE',  ( 0.4303681241740789920, -0.1153557615287144622, -1.934055118110236338 ) ) ;
#259 = CARTESIAN_POINT ( 'NONE',  ( -0.3233561589689049609, -0.1867299569291588357, -3.115157480314960647 ) ) ;
#260 = DIRECTION ( 'NONE',  ( 0.000000000000000000, -0.4702444477782212195, 0.8825362085114445421 ) ) ;
#261 = CARTESIAN_POINT ( 'NONE',  ( 0.2965233727166233790, 0.3524965443697388734, 0.1771653543307087630 ) ) ;
#262 = DIRECTION ( 'NONE',  ( 0.8660254037844385966, 0.4999999999999998335, 0.000000000000000000 ) ) ;
#263 = ORIENTED_EDGE ( 'NONE', *, *, #3631, .F. ) ;
#264 = DIRECTION ( 'NONE',  ( -0.000000000000000000, -1.000000000000000000, -0.000000000000000000 ) ) ;
#265 = CIRCLE ( 'NONE', #4300, 0.01377952755905510404 ) ;
#266 = CIRCLE ( 'NONE', #11488, 0.4692913385826771866 ) ;
#267 = EDGE_CURVE ( 'NONE', #4877, #9806, #20517, .T. ) ;
#268 = ORIENTED_EDGE ( 'NONE', *, *, #11086, .F. ) ;
#269 = CARTESIAN_POINT ( 'NONE',  ( 0.3751294191746885609, 0.2999672986753447734, 0.2362204724409446843 ) ) ;
#270 = APPLICATION_PROTOCOL_DEFINITION ( 'draft international standard', 'automotive_design', 1998, #14720 ) ;
#271 = CARTESIAN_POINT ( 'NONE',  ( 0.5118110236220472231, 0.03349795313260757468, 1.766732283464566899 ) ) ;
#272 = EDGE_CURVE ( 'NONE', #27250, #26868, #24521, .T. ) ;
#273 = AXIS2_PLACEMENT_3D ( 'NONE', #1316, #18082, #27170 ) ;
#274 = ORIENTED_EDGE ( 'NONE', *, *, #6413, .T. ) ;
#275 = ORIENTED_EDGE ( 'NONE', *, *, #12081, .F. ) ;
#276 = ORIENTED_EDGE ( 'NONE', *, *, #1809, .T. ) ;
#277 = CARTESIAN_POINT ( 'NONE',  ( 0.2362439534887500470, 0.2693339498142248156, -3.115157480314960647 ) ) ;
#279 = DIRECTION ( 'NONE',  ( 0.000000000000000000, 1.000000000000000000, 0.000000000000000000 ) ) ;
#278 = ( REPRESENTATION_RELATIONSHIP ('NONE','NONE', #12434, #6338 ) REPRESENTATION_RELATIONSHIP_WITH_TRANSFORMATION ( #9729 )SHAPE_REPRESENTATION_RELATIONSHIP( ) ) ;
#280 = VERTEX_POINT ( 'NONE', #5695 ) ;
#281 = FACE_OUTER_BOUND ( 'NONE', #3824, .T. ) ;
#282 = DIRECTION ( 'NONE',  ( -5.737213000000000442E-16, 1.000000000000000000, -1.224646799147353207E-16 ) ) ;
#283 = CARTESIAN_POINT ( 'NONE',  ( 0.2521176338356670432, 0.2211428102655656758, 1.953740157480315043 ) ) ;
#284 = EDGE_CURVE ( 'NONE', #11054, #21365, #5605, .T. ) ;
#285 = VERTEX_POINT ( 'NONE', #25460 ) ;
#286 = B_SPLINE_CURVE_WITH_KNOTS ( 'NONE', 3,
 ( #23808, #10659, #8682, #25644, #1905, #25921 ),
 .UNSPECIFIED., .F., .F.,
 ( 4, 2, 4 ),
 ( 0.7157687286427140139, 0.7172350147555670574, 0.7187013008684199900 ),
 .UNSPECIFIED. ) ;
#287 = LINE ( 'NONE', #8993, #4640 ) ;
#288 = VECTOR ( 'NONE', #25733, 39.37007874015748143 ) ;
#289 = ORIENTED_EDGE ( 'NONE', *, *, #13370, .F. ) ;
#290 = VERTEX_POINT ( 'NONE', #22923 ) ;
#291 = ORIENTED_EDGE ( 'NONE', *, *, #20836, .F. ) ;
#292 = DIRECTION ( 'NONE',  ( -1.000000000000000000, -7.017815999999999636E-18, 0.000000000000000000 ) ) ;
#293 = CARTESIAN_POINT ( 'NONE',  ( 0.6947676139410623453, 0.7729092381583980709, -0.02125091332446964881 ) ) ;
#294 = ORIENTED_EDGE ( 'NONE', *, *, #2324, .F. ) ;
#295 = VECTOR ( 'NONE', #17634, 39.37007874015748143 ) ;
#296 = EDGE_CURVE ( 'NONE', #10766, #14592, #15963, .T. ) ;
#297 = CARTESIAN_POINT ( 'NONE',  ( -0.6708219662590964028, -0.1536294932067021612, 0.1322818203437344520 ) ) ;
#298 = EDGE_CURVE ( 'NONE', #7459, #10848, #1546, .T. ) ;
#299 = CARTESIAN_POINT ( 'NONE',  ( -0.5190862322091315262, -0.1177929122753175184, 0.3401574803149606252 ) ) ;
#300 = ADVANCED_FACE ( 'NONE', ( #3258 ), #20928, .T. ) ;
#301 = ORIENTED_EDGE ( 'NONE', *, *, #18506, .T. ) ;
#302 = AXIS2_PLACEMENT_3D ( 'NONE', #2958, #11178, #15703 ) ;
#303 = DIRECTION ( 'NONE',  ( 0.000000000000000000, 0.000000000000000000, -1.000000000000000000 ) ) ;
#304 = B_SPLINE_CURVE_WITH_KNOTS ( 'NONE', 3,
 ( #11360, #4990, #21548, #4455 ),
 .UNSPECIFIED., .F., .F.,
 ( 4, 4 ),
 ( 1.743059029969425078, 1.744705333033724992 ),
 .UNSPECIFIED. ) ;
#305 = VECTOR ( 'NONE', #25355, 39.37007874015748854 ) ;
#306 = CARTESIAN_POINT ( 'NONE',  ( 0.07870736599818350943, 0.1968503937007873850, -3.212150913008773312 ) ) ;
#307 = ORIENTED_EDGE ( 'NONE', *, *, #13471, .F. ) ;
#308 = DIRECTION ( 'NONE',  ( 0.7660444431189782355, 0.6427876096865391409, 0.000000000000000000 ) ) ;
#309 = ( CONVERSION_BASED_UNIT ( 'INCH', #689 ) LENGTH_UNIT ( ) NAMED_UNIT ( #9238 ) ) ;
#310 = CARTESIAN_POINT ( 'NONE',  ( 0.3362554559023149814, -0.1141145734059788724, 1.953740157480315043 ) ) ;
#311 = ORIENTED_EDGE ( 'NONE', *, *, #16319, .F. ) ;
#312 = DIRECTION ( 'NONE',  ( 0.000000000000000000, 0.000000000000000000, 1.000000000000000000 ) ) ;
#313 = DIRECTION ( 'NONE',  ( -1.000000000000000000, 0.000000000000000000, 0.000000000000000000 ) ) ;
#314 = PLANE ( 'NONE',  #8850 ) ;
#315 = FACE_OUTER_BOUND ( 'NONE', #4485, .T. ) ;
#316 = ORIENTED_EDGE ( 'NONE', *, *, #13974, .F. ) ;
#317 = CARTESIAN_POINT ( 'NONE',  ( 0.4783323773986625782, 0.2762247810518427271, 0.9399606299212598381 ) ) ;
#318 = ORIENTED_EDGE ( 'NONE', *, *, #26206, .F. ) ;
#319 = DIRECTION ( 'NONE',  ( 1.000000000000000000, 0.000000000000000000, 0.000000000000000000 ) ) ;
#320 = ORIENTED_EDGE ( 'NONE', *, *, #13672, .F. ) ;
#321 = VECTOR ( 'NONE', #12149, 39.37007874015748143 ) ;
#322 = FACE_OUTER_BOUND ( 'NONE', #12534, .T. ) ;
#323 = CARTESIAN_POINT ( 'NONE',  ( -0.4126915023524561632, -0.2375990495015092296, 0.2330651858026694390 ) ) ;
#324 = AXIS2_PLACEMENT_3D ( 'NONE', #9492, #22508, #24756 ) ;
#325 = CARTESIAN_POINT ( 'NONE',  ( -0.1716509673353403542, -0.4704508543867079173, 0.09684874903502814492 ) ) ;
#326 = CARTESIAN_POINT ( 'NONE',  ( -0.1196556571310431333, -0.3272932875252256291, 0.1166443193928402983 ) ) ;
#327 = CARTESIAN_POINT ( 'NONE',  ( 0.5692936381926190226, -0.3294684677443725507, 0.2081850588275903358 ) ) ;
#328 = FACE_OUTER_BOUND ( 'NONE', #1258, .T. ) ;
#329 = EDGE_CURVE ( 'NONE', #8378, #18994, #15536, .T. ) ;
#330 = ORIENTED_EDGE ( 'NONE', *, *, #18348, .T. ) ;
#331 = CARTESIAN_POINT ( 'NONE',  ( 0.000000000000000000, 0.000000000000000000, -0.2342519685039370358 ) ) ;
#332 = CARTESIAN_POINT ( 'NONE',  ( -0.2529800193559212929, 0.5131133041954029084, 0.9399606299212598381 ) ) ;
#333 = VERTEX_POINT ( 'NONE', #9774 ) ;
#334 = CARTESIAN_POINT ( 'NONE',  ( -0.5118110236220472231, 0.000000000000000000, 1.953740157480315043 ) ) ;
#335 = CARTESIAN_POINT ( 'NONE',  ( 0.000000000000000000, 0.000000000000000000, 0.2362204724409449064 ) ) ;
#336 = AXIS2_PLACEMENT_3D ( 'NONE', #6221, #5940, #1966 ) ;
#337 = CONICAL_SURFACE ( 'NONE', #25107, 0.06200787401574805319, 1.029744258088332254 ) ;
#338 = ORIENTED_EDGE ( 'NONE', *, *, #23140, .F. ) ;
#339 = VERTEX_POINT ( 'NONE', #12317 ) ;
#340 = CIRCLE ( 'NONE', #27828, 0.1181102362204724532 ) ;
#341 = B_SPLINE_CURVE_WITH_KNOTS ( 'NONE', 3,
 ( #20281, #13782, #13925, #26772, #18280, #24375, #3448, #26627, #7564, #796, #2888, #16049, #22829 ),
 .UNSPECIFIED., .F., .F.,
 ( 4, 3, 3, 3, 4 ),
 ( 0.01512411120486024073, 0.01814893344583978774, 0.02117375568681436129, 0.02419857792778855668, 0.02712411120487693422 ),
 .UNSPECIFIED. ) ;
#342 = CARTESIAN_POINT ( 'NONE',  ( -0.4333973147258542991, -0.2509079296564011852, 0.09685039370078740717 ) ) ;
#343 = DIRECTION ( 'NONE',  ( 0.000000000000000000, 1.000000000000000000, 0.000000000000000000 ) ) ;
#344 = ADVANCED_FACE ( 'NONE', ( #1581, #10184 ), #10334, .T. ) ;
#345 = ORIENTED_EDGE ( 'NONE', *, *, #3993, .T. ) ;
#346 = CARTESIAN_POINT ( 'NONE',  ( 0.06200787401574806013, 0.000000000000000000, 0.7844728274238290666 ) ) ;
#347 = ORIENTED_EDGE ( 'NONE', *, *, #11626, .F. ) ;
#348 = EDGE_CURVE ( 'NONE', #27369, #9997, #27259, .T. ) ;
#349 = LINE ( 'NONE', #4682, #16207 ) ;
#350 = CARTESIAN_POINT ( 'NONE',  ( 0.6996455634132897616, -0.1588938903156011662, 0.1601585119484411623 ) ) ;
#351 = CARTESIAN_POINT ( 'NONE',  ( 0.1532705055535415473, -0.8125630895486949390, -0.04838628589907047889 ) ) ;
#352 = FILL_AREA_STYLE_COLOUR ( '', #20221 ) ;
#353 = DIRECTION ( 'NONE',  ( -0.000000000000000000, 1.000000000000000000, -0.000000000000000000 ) ) ;
#354 = CARTESIAN_POINT ( 'NONE',  ( 0.1718374205099799101, -0.4703827404237102550, 0.09685039370078740717 ) ) ;
#355 = EDGE_CURVE ( 'NONE', #14294, #8859, #26577, .T. ) ;
#356 = ADVANCED_FACE ( 'NONE', ( #15159 ), #8639, .T. ) ;
#357 = ORIENTED_EDGE ( 'NONE', *, *, #17696, .F. ) ;
#358 = DIRECTION ( 'NONE',  ( 0.000000000000000000, 0.000000000000000000, -1.000000000000000000 ) ) ;
#359 = DIRECTION ( 'NONE',  ( -1.000000000000000000, -1.224646799147356165E-16, 0.000000000000000000 ) ) ;
#360 = CARTESIAN_POINT ( 'NONE',  ( 0.4423390553432928751, 0.2180862235769577551, -1.550196850393700920 ) ) ;
#361 = CARTESIAN_POINT ( 'NONE',  ( -0.4438564651657384008, -0.1188866373884874261, -1.928289503579162067 ) ) ;
#362 = CARTESIAN_POINT ( 'NONE',  ( 0.09842519685039358146, 0.2991866959364303802, -3.548228346456693050 ) ) ;
#363 = DIRECTION ( 'NONE',  ( 0.000000000000000000, 0.000000000000000000, -1.000000000000000000 ) ) ;
#364 = LINE ( 'NONE', #17572, #14246 ) ;
#365 = CARTESIAN_POINT ( 'NONE',  ( 0.3411065095061437402, 0.06065137456822566192, 0.1377952755905510474 ) ) ;
#366 = DIRECTION ( 'NONE',  ( 0.000000000000000000, 1.000000000000000000, 0.000000000000000000 ) ) ;
#367 = AXIS2_PLACEMENT_3D ( 'NONE', #8300, #14535, #6190 ) ;
#368 = ORIENTED_EDGE ( 'NONE', *, *, #7108, .F. ) ;
#369 = CARTESIAN_POINT ( 'NONE',  ( -0.03532354024591771724, -0.6299212598425195653, 0.6299212598425196763 ) ) ;
#370 = ORIENTED_EDGE ( 'NONE', *, *, #13419, .F. ) ;
#371 = CARTESIAN_POINT ( 'NONE',  ( -0.7635713814939685262, 0.2506761191097937047, -0.2749095812957952911 ) ) ;
#372 = VERTEX_POINT ( 'NONE', #12604 ) ;
#373 = EDGE_CURVE ( 'NONE', #24937, #5795, #15104, .T. ) ;
#374 = AXIS2_PLACEMENT_3D ( 'NONE', #10936, #6568, #8678 ) ;
#375 = DIRECTION ( 'NONE',  ( -0.5000000010362850578, -0.8660254031861391866, -1.060575237992201443E-16 ) ) ;
#376 = CYLINDRICAL_SURFACE ( 'NONE', #17012, 0.4842519685039370358 ) ;
#377 = LINE ( 'NONE', #8956, #9112 ) ;
#378 = CARTESIAN_POINT ( 'NONE',  ( 0.000000000000000000, 0.07874015746264864668, 0.000000000000000000 ) ) ;
#379 = CARTESIAN_POINT ( 'NONE',  ( -0.7874015748031496509, 0.8628702403565570167, -0.3208896918748870286 ) ) ;
#380 = EDGE_CURVE ( 'NONE', #22824, #12297, #25600, .T. ) ;
#381 = CARTESIAN_POINT ( 'NONE',  ( 0.05811992390581651596, -0.4417530401346463909, -1.934055118110236560 ) ) ;
#382 = CARTESIAN_POINT ( 'NONE',  ( -0.3349073414798507953, 0.1651192144506273274, -3.115157480314960647 ) ) ;
#383 = EDGE_CURVE ( 'NONE', #23520, #15671, #17764, .T. ) ;
#384 = SURFACE_SIDE_STYLE ('',( #2200 ) ) ;
#385 = CARTESIAN_POINT ( 'NONE',  ( -0.2230788859036006988, 0.2650812153444457309, 0.1276989850646860214 ) ) ;
#386 = VECTOR ( 'NONE', #3077, 39.37007874015748143 ) ;
#387 = ORIENTED_EDGE ( 'NONE', *, *, #3265, .F. ) ;
#388 = DIRECTION ( 'NONE',  ( 0.000000000000000000, 0.000000000000000000, -1.000000000000000000 ) ) ;
#389 = DIMENSIONAL_EXPONENTS ( 1.000000000000000000, 0.000000000000000000, 0.000000000000000000, 0.000000000000000000, 0.000000000000000000, 0.000000000000000000, 0.000000000000000000 ) ;
#390 = AXIS2_PLACEMENT_3D ( 'NONE', #12393, #16488, #25245 ) ;
#391 = AXIS2_PLACEMENT_3D ( 'NONE', #18400, #12341, #14636 ) ;
#392 = ORIENTED_EDGE ( 'NONE', *, *, #12058, .F. ) ;
#393 = DIRECTION ( 'NONE',  ( 0.6427876096865396960, 0.7660444431189776804, -0.000000000000000000 ) ) ;
#394 = LINE ( 'NONE', #15375, #16281 ) ;
#395 = DIRECTION ( 'NONE',  ( 1.000000000000000000, 0.000000000000000000, 0.000000000000000000 ) ) ;
#396 = CARTESIAN_POINT ( 'NONE',  ( -0.1649135259617042215, 0.4856708409200647392, 1.766732283464566899 ) ) ;
#397 = B_SPLINE_CURVE_WITH_KNOTS ( 'NONE', 3,
 ( #22454, #26273, #15820, #17525, #20191, #11434, #11714, #3081 ),
 .UNSPECIFIED., .F., .F.,
 ( 4, 2, 2, 4 ),
 ( 0.5000000000000000000, 0.7499999999999997780, 0.8749999999999998890, 1.000000000000000000 ),
 .UNSPECIFIED. ) ;
#398 = DIRECTION ( 'NONE',  ( -1.000000000000000000, 0.000000000000000000, 0.000000000000000000 ) ) ;
#399 = ORIENTED_EDGE ( 'NONE', *, *, #24266, .F. ) ;
#400 = CARTESIAN_POINT ( 'NONE',  ( 0.3349073414798194315, 0.1651192144506304638, -3.115157480314960647 ) ) ;
#401 = VERTEX_POINT ( 'NONE', #26015 ) ;
#402 = CYLINDRICAL_SURFACE ( 'NONE', #15048, 0.3149606299212598381 ) ;
#403 = CARTESIAN_POINT ( 'NONE',  ( 0.000000000000000000, 0.3543307086614173040, 0.000000000000000000 ) ) ;
#404 = VECTOR ( 'NONE', #11672, 39.37007874015748143 ) ;
#405 = CARTESIAN_POINT ( 'NONE',  ( -0.02190250779245987017, -0.3346456692913385988, 1.953740157480315043 ) ) ;
#406 = ORIENTED_EDGE ( 'NONE', *, *, #12519, .T. ) ;
#407 = ORIENTED_EDGE ( 'NONE', *, *, #26451, .F. ) ;
#408 = ADVANCED_FACE ( 'NONE', ( #17123 ), #19236, .F. ) ;
#409 = AXIS2_PLACEMENT_3D ( 'NONE', #960, #9547, #5473 ) ;
#410 = DIRECTION ( 'NONE',  ( 0.000000000000000000, 0.000000000000000000, 1.000000000000000000 ) ) ;
#411 = ( GEOMETRIC_REPRESENTATION_CONTEXT ( 3 ) GLOBAL_UNCERTAINTY_ASSIGNED_CONTEXT ( ( #18335 ) ) GLOBAL_UNIT_ASSIGNED_CONTEXT ( ( #27464, #8113, #23091 ) ) REPRESENTATION_CONTEXT ( 'NONE', 'WORKASPACE' ) ) ;
#412 = ORIENTED_EDGE ( 'NONE', *, *, #25098, .T. ) ;
#413 = ORIENTED_EDGE ( 'NONE', *, *, #20952, .T. ) ;
#414 = ORIENTED_EDGE ( 'NONE', *, *, #16074, .T. ) ;
#415 = CARTESIAN_POINT ( 'NONE',  ( 0.000000000000000000, 0.1574803148899641958, 0.000000000000000000 ) ) ;
#416 = EDGE_CURVE ( 'NONE', #7640, #15191, #10471, .T. ) ;
#417 = DIRECTION ( 'NONE',  ( -0.000000000000000000, -0.000000000000000000, -1.000000000000000000 ) ) ;
#418 = DIRECTION ( 'NONE',  ( -1.000000000000000000, 0.000000000000000000, 0.000000000000000000 ) ) ;
#419 = CARTESIAN_POINT ( 'NONE',  ( 0.6015839972843660677, 0.9161431246486984037, -0.1460888818946199375 ) ) ;
#420 = CARTESIAN_POINT ( 'NONE',  ( 0.3002886982018041495, -0.1727973894384573217, 0.1478915661278440430 ) ) ;
#421 = TOROIDAL_SURFACE ( 'NONE', #8530, 0.4232283464566928832, 0.07677165354330708902 ) ;
#422 = CARTESIAN_POINT ( 'NONE',  ( -0.5188388941967637669, -0.1188778293835246053, 0.3401591244667909186 ) ) ;
#423 = CIRCLE ( 'NONE', #2649, 0.6881889763779527325 ) ;
#424 = CARTESIAN_POINT ( 'NONE',  ( -0.3991696156513551141, 0.4760540497243913594, 0.09684793308443542803 ) ) ;
#425 = AXIS2_PLACEMENT_3D ( 'NONE', #17792, #8636, #2410 ) ;
#426 = FACE_BOUND ( 'NONE', #2820, .T. ) ;
#427 = LINE ( 'NONE', #11141, #5205 ) ;
#428 = ORIENTED_EDGE ( 'NONE', *, *, #19664, .T. ) ;
#429 = CIRCLE ( 'NONE', #27509, 0.07677362204724409722 ) ;
#430 = DIRECTION ( 'NONE',  ( -1.000000000000000000, 0.000000000000000000, 0.000000000000000000 ) ) ;
#431 = CARTESIAN_POINT ( 'NONE',  ( 0.2161875334157469797, -0.2816963220976381743, 1.953740157480315043 ) ) ;
#432 = ORIENTED_EDGE ( 'NONE', *, *, #5914, .T. ) ;
#433 = DIRECTION ( 'NONE',  ( 1.000000000000000000, 0.000000000000000000, 0.000000000000000000 ) ) ;
#434 = DIRECTION ( 'NONE',  ( -1.000000000000000000, 0.000000000000000000, 0.000000000000000000 ) ) ;
#435 = DIRECTION ( 'NONE',  ( 0.000000000000000000, -1.000000000000000000, 0.000000000000000000 ) ) ;
#436 = CARTESIAN_POINT ( 'NONE',  ( 0.000000000000000000, 0.4724409448818898127, 0.000000000000000000 ) ) ;
#437 = EDGE_LOOP ( 'NONE', ( #11123, #6651, #25287, #3751, #12023, #11943, #16300, #8034, #5039, #15886, #22940, #20148, #24795, #15480 ) ) ;
#438 = CARTESIAN_POINT ( 'NONE',  ( -0.1775991818008579581, 0.5230301363771275858, 0.9399606299212598381 ) ) ;
#439 = EDGE_LOOP ( 'NONE', ( #13382, #10561, #4608, #2891 ) ) ;
#440 = EDGE_CURVE ( 'NONE', #19589, #20556, #3761, .T. ) ;
#441 = DIRECTION ( 'NONE',  ( 1.000000000000000000, 0.000000000000000000, 0.000000000000000000 ) ) ;
#442 = ORIENTED_EDGE ( 'NONE', *, *, #8042, .F. ) ;
#443 = CARTESIAN_POINT ( 'NONE',  ( 0.3066721922917531873, -3.755651186775971117E-17, -0.05856299212598425896 ) ) ;
#444 = DIRECTION ( 'NONE',  ( 0.000000000000000000, 0.000000000000000000, 1.000000000000000000 ) ) ;
#445 = VECTOR ( 'NONE', #20789, 39.37007874015748854 ) ;
#446 = FACE_BOUND ( 'NONE', #5587, .T. ) ;
#447 = FACE_OUTER_BOUND ( 'NONE', #2356, .T. ) ;
#448 = DIRECTION ( 'NONE',  ( 0.000000000000000000, 1.000000000000000000, 0.000000000000000000 ) ) ;
#449 = CARTESIAN_POINT ( 'NONE',  ( 0.3665264996331779601, -0.2116141732283464416, 0.06102165354330708891 ) ) ;
#450 = DIRECTION ( 'NONE',  ( 0.000000000000000000, 0.000000000000000000, 1.000000000000000000 ) ) ;
#451 = CARTESIAN_POINT ( 'NONE',  ( 0.0003854097503897235258, 0.4692912202195575477, 0.07637630773773071424 ) ) ;
#452 = CARTESIAN_POINT ( 'NONE',  ( -0.3040421205569480145, 1.249037478091203024, -0.7140903627573721435 ) ) ;
#453 = CARTESIAN_POINT ( 'NONE',  ( -0.2860899518037610667, -0.4954156765914530247, 0.9399606299212598381 ) ) ;
#454 = DIRECTION ( 'NONE',  ( -0.9396926207859082059, 0.3420201433256690460, 0.000000000000000000 ) ) ;
#455 = EDGE_LOOP ( 'NONE', ( #21563, #19160, #191, #7147 ) ) ;
#456 = CARTESIAN_POINT ( 'NONE',  ( -0.4684132450478830645, -0.1062614382955276715, 0.2362204724409449619 ) ) ;
#457 = AXIS2_PLACEMENT_3D ( 'NONE', #11632, #18253, #20541 ) ;
#458 = AXIS2_PLACEMENT_3D ( 'NONE', #6185, #12523, #23694 ) ;
#459 = ORIENTED_EDGE ( 'NONE', *, *, #5759, .F. ) ;
#460 = CARTESIAN_POINT ( 'NONE',  ( -0.5190862322091315262, -0.1177929122753175184, 0.3401574803149606252 ) ) ;
#461 = DIRECTION ( 'NONE',  ( -1.000000000000000000, 0.000000000000000000, 0.000000000000000000 ) ) ;
#462 = CARTESIAN_POINT ( 'NONE',  ( 0.4887136534578185310, -0.1122103150229527835, 0.1643955689280507948 ) ) ;
#463 = ORIENTED_EDGE ( 'NONE', *, *, #26682, .F. ) ;
#464 = ADVANCED_FACE ( 'NONE', ( #6671 ), #22286, .T. ) ;
#465 = DIRECTION ( 'NONE',  ( 1.000000000000000000, 0.000000000000000000, 0.000000000000000000 ) ) ;
#466 = ORIENTED_EDGE ( 'NONE', *, *, #18480, .T. ) ;
#467 = CARTESIAN_POINT ( 'NONE',  ( -0.2981382804007346454, -0.6202561546315846774, 0.1322818203437346463 ) ) ;
#468 = CARTESIAN_POINT ( 'NONE',  ( 0.1525037638700916243, 0.2314035372547586233, -0.4381595109572587465 ) ) ;
#469 = CARTESIAN_POINT ( 'NONE',  ( 0.1120675189988346587, -0.7410715175625038897, 0.001857066358701141805 ) ) ;
#470 = CIRCLE ( 'NONE', #7684, 0.6889763779527560139 ) ;
#471 = DIRECTION ( 'NONE',  ( -0.9848077530122080203, 0.1736481776669311083, 0.000000000000000000 ) ) ;
#472 = AXIS2_PLACEMENT_3D ( 'NONE', #24555, #16101, #700 ) ;
#473 = DIRECTION ( 'NONE',  ( 0.000000000000000000, 0.000000000000000000, 1.000000000000000000 ) ) ;
#474 = CARTESIAN_POINT ( 'NONE',  ( 0.1710938124795997883, -0.4706537664821763833, 0.09684793308443542803 ) ) ;
#475 = ORIENTED_EDGE ( 'NONE', *, *, #3137, .F. ) ;
#476 = CARTESIAN_POINT ( 'NONE',  ( -0.1968503937007874127, -0.07874015748031495954, 0.04546065111729338803 ) ) ;
#477 = CARTESIAN_POINT ( 'NONE',  ( -0.03220957031754079214, -0.4921259842519685179, -1.550196850393700920 ) ) ;
#478 = VERTEX_POINT ( 'NONE', #6529 ) ;
#479 = CYLINDRICAL_SURFACE ( 'NONE', #571, 0.5570866141732283561 ) ;
#480 = AXIS2_PLACEMENT_3D ( 'NONE', #1585, #2519, #13258 ) ;
#481 = CARTESIAN_POINT ( 'NONE',  ( 0.1648264847746512829, -0.4857053587577857545, -1.550196850393700920 ) ) ;
#482 = CARTESIAN_POINT ( 'NONE',  ( 1.197070535079588716, 0.4724409448818898127, -1.315180771300060503 ) ) ;
#483 = ADVANCED_FACE ( 'NONE', ( #19377 ), #13015, .T. ) ;
#484 = CARTESIAN_POINT ( 'NONE',  ( 0.1706130639257694703, -0.4670119966460608563, 0.1140743250952255261 ) ) ;
#485 = CARTESIAN_POINT ( 'NONE',  ( -0.6370261810203012853, -0.05236013009244417510, -0.08009157605482203346 ) ) ;
#486 = DIRECTION ( 'NONE',  ( 1.000000000000000000, 0.000000000000000000, 0.000000000000000000 ) ) ;
#487 = PRESENTATION_STYLE_ASSIGNMENT (( #238 ) ) ;
#488 = ORIENTED_EDGE ( 'NONE', *, *, #21767, .T. ) ;
#489 = CIRCLE ( 'NONE', #20321, 0.5322834645669292097 ) ;
#490 = CARTESIAN_POINT ( 'NONE',  ( -0.6614173228346456046, 0.000000000000000000, -0.2480314960629921295 ) ) ;
#491 = ADVANCED_FACE ( 'NONE', ( #21504 ), #18663, .F. ) ;
#492 = FACE_BOUND ( 'NONE', #4958, .T. ) ;
#493 = EDGE_LOOP ( 'NONE', ( #11745, #14981, #2623, #22261 ) ) ;
#494 = CARTESIAN_POINT ( 'NONE',  ( -0.03532354024591775193, -0.07677165354330710290, 0.000000000000000000 ) ) ;
#495 = DIRECTION ( 'NONE',  ( 0.000000000000000000, 0.000000000000000000, 1.000000000000000000 ) ) ;
#496 = VERTEX_POINT ( 'NONE', #19091 ) ;
#497 = CIRCLE ( 'NONE', #20352, 0.4692913385826771866 ) ;
#498 = DIRECTION ( 'NONE',  ( 0.000000000000000000, 1.000000000000000000, 0.000000000000000000 ) ) ;
#499 = DIRECTION ( 'NONE',  ( 0.000000000000000000, 0.000000000000000000, -1.000000000000000000 ) ) ;
#500 = B_SPLINE_CURVE_WITH_KNOTS ( 'NONE', 3,
 ( #10699, #21447, #8173, #14554, #4212, #19314, #8315, #6201, #17200, #2088 ),
 .UNSPECIFIED., .F., .F.,
 ( 4, 2, 2, 2, 4 ),
 ( 0.000000000000000000, 0.2500000000000000000, 0.5000000000000000000, 0.7500000000000000000, 1.000000000000000000 ),
 .UNSPECIFIED. ) ;
#501 = CARTESIAN_POINT ( 'NONE',  ( -0.3355349563089153886, 0.1597155962083088576, 0.2362204724409449064 ) ) ;
#502 = CARTESIAN_POINT ( 'NONE',  ( 0.2712680014829234043, -0.3534612032201311371, -1.934055118110236338 ) ) ;
#503 = LINE ( 'NONE', #20402, #13869 ) ;
#504 = LINE ( 'NONE', #11227, #20509 ) ;
#505 = CARTESIAN_POINT ( 'NONE',  ( 0.6512499169092683671, 0.1155267097728963771, 0.1926811207759472899 ) ) ;
#506 = ORIENTED_EDGE ( 'NONE', *, *, #4372, .T. ) ;
#507 = DIRECTION ( 'NONE',  ( 0.000000000000000000, 0.000000000000000000, -1.000000000000000000 ) ) ;
#508 = AXIS2_PLACEMENT_3D ( 'NONE', #15619, #21831, #3001 ) ;
#509 = ADVANCED_FACE ( 'NONE', ( #25741, #6394 ), #27730, .T. ) ;
#510 = PRESENTATION_LAYER_ASSIGNMENT (  '', '', ( #7735 ) ) ;
#511 = VECTOR ( 'NONE', #19555, 39.37007874015748143 ) ;
#512 = ORIENTED_EDGE ( 'NONE', *, *, #14893, .F. ) ;
#513 = ORIENTED_EDGE ( 'NONE', *, *, #2642, .T. ) ;
#514 = CARTESIAN_POINT ( 'NONE',  ( 7.232166136913317628E-17, 0.07874015746264864668, -0.5905511811200284678 ) ) ;
#515 = DIRECTION ( 'NONE',  ( 0.000000000000000000, 1.000000000000000000, 0.000000000000000000 ) ) ;
#516 = SHAPE_DEFINITION_REPRESENTATION ( #3947, #26684 ) ;
#517 = CARTESIAN_POINT ( 'NONE',  ( -0.4600326175560697783, 0.2268096725222554233, 1.747047244094488194 ) ) ;
#518 = ADVANCED_FACE ( 'NONE', ( #21226 ), #21837, .T. ) ;
#519 = FACE_OUTER_BOUND ( 'NONE', #10794, .T. ) ;
#520 = EDGE_LOOP ( 'NONE', ( #11696, #24909 ) ) ;
#521 = CARTESIAN_POINT ( 'NONE',  ( 0.1867299569291587802, -0.3233561589689049609, -3.115157480314960647 ) ) ;
#522 = EDGE_CURVE ( 'NONE', #3990, #21275, #23634, .T. ) ;
#523 = EDGE_LOOP ( 'NONE', ( #21704, #21460, #12292, #1622, #7292, #18239 ) ) ;
#524 = LINE ( 'NONE', #2219, #4201 ) ;
#525 = CARTESIAN_POINT ( 'NONE',  ( 0.1490609433494345937, 0.2434005097105403082, -0.4121204548294903347 ) ) ;
#526 = CARTESIAN_POINT ( 'NONE',  ( -0.3175540113612211890, 0.1078280746903930443, 1.953740157480315043 ) ) ;
#527 = VERTEX_POINT ( 'NONE', #4408 ) ;
#528 = EDGE_LOOP ( 'NONE', ( #9986, #24877, #1531, #26427 ) ) ;
#529 = AXIS2_PLACEMENT_3D ( 'NONE', #1743, #21245, #23088 ) ;
#530 = CARTESIAN_POINT ( 'NONE',  ( 0.000000000000000000, 0.000000000000000000, -3.110236220451535694 ) ) ;
#531 = ORIENTED_EDGE ( 'NONE', *, *, #2877, .F. ) ;
#532 = B_SPLINE_CURVE_WITH_KNOTS ( 'NONE', 3,
 ( #24989, #10725, #23173, #16808 ),
 .UNSPECIFIED., .F., .F.,
 ( 4, 4 ),
 ( 0.9895101543494979612, 0.9911564574137969874 ),
 .UNSPECIFIED. ) ;
#533 = ORIENTED_EDGE ( 'NONE', *, *, #26084, .F. ) ;
#534 = ORIENTED_EDGE ( 'NONE', *, *, #21353, .T. ) ;
#535 = CARTESIAN_POINT ( 'NONE',  ( -0.04840761057735708250, 0.1968503937007874127, -3.611172162805734942 ) ) ;
#536 = CIRCLE ( 'NONE', #16320, 0.3937007874015748254 ) ;
#537 = CARTESIAN_POINT ( 'NONE',  ( 0.3843128886798082844, 0.1691648655974895832, -0.07874015748031495954 ) ) ;
#538 = CARTESIAN_POINT ( 'NONE',  ( -0.07874015748031502893, 0.1968503937007874127, -3.272637795275590733 ) ) ;
#539 = CARTESIAN_POINT ( 'NONE',  ( 0.7732217274635454496, 0.5458307047179269400, 0.1151719495065113841 ) ) ;
#540 = EDGE_LOOP ( 'NONE', ( #5491, #24841, #13223, #6608 ) ) ;
#541 = DIRECTION ( 'NONE',  ( 1.000000000000000000, 0.000000000000000000, 0.000000000000000000 ) ) ;
#542 = CARTESIAN_POINT ( 'NONE',  ( -0.3074993854542729665, -0.1775730735577446262, 1.953740157480315043 ) ) ;
#543 = CARTESIAN_POINT ( 'NONE',  ( -0.0006620872580281702332, 0.5229309616561139684, 0.3331434174598592590 ) ) ;
#544 = EDGE_CURVE ( 'NONE', #25079, #10563, #9634, .T. ) ;
#545 = CIRCLE ( 'NONE', #13618, 0.01377952755905510404 ) ;
#546 = DIRECTION ( 'NONE',  ( 1.000000000000000000, 0.000000000000000000, 0.000000000000000000 ) ) ;
#547 = CARTESIAN_POINT ( 'NONE',  ( -0.4210617728863489950, -0.2437762437896736079, 0.2467937633087636806 ) ) ;
#548 = CARTESIAN_POINT ( 'NONE',  ( 0.0006679551606482677165, 0.5322830454629158270, 0.1322834645669291320 ) ) ;
#549 = ADVANCED_FACE ( 'NONE', ( #4668 ), #4259, .T. ) ;
#550 = VERTEX_POINT ( 'NONE', #15439 ) ;
#551 = CARTESIAN_POINT ( 'NONE',  ( 0.4061284506584276199, -0.2351468520616558922, 0.07637795275590551769 ) ) ;
#552 = ORIENTED_EDGE ( 'NONE', *, *, #3585, .T. ) ;
#553 = CARTESIAN_POINT ( 'NONE',  ( -0.2956505864974144360, 0.3532288989643737054, 0.1903859677777559323 ) ) ;
#554 = ORIENTED_EDGE ( 'NONE', *, *, #13765, .T. ) ;
#555 = CARTESIAN_POINT ( 'NONE',  ( -0.4792984784078200833, 0.08391448672304414880, 0.09284957166327162392 ) ) ;
#556 = EDGE_CURVE ( 'NONE', #4928, #5829, #1626, .T. ) ;
#557 = ORIENTED_EDGE ( 'NONE', *, *, #23990, .T. ) ;
#558 = DIRECTION ( 'NONE',  ( 1.000000000000000000, 0.000000000000000000, 0.000000000000000000 ) ) ;
#559 = CARTESIAN_POINT ( 'NONE',  ( -0.2420394123212937232, 0.2892587550802429575, 0.1992125984251968684 ) ) ;
#560 = ORIENTED_EDGE ( 'NONE', *, *, #19691, .F. ) ;
#561 = CARTESIAN_POINT ( 'NONE',  ( 0.4152525734085952824, 0.3642352168757231889, 0.9399606299212598381 ) ) ;
#562 = FACE_OUTER_BOUND ( 'NONE', #19020, .T. ) ;
#563 = ORIENTED_EDGE ( 'NONE', *, *, #5290, .F. ) ;
#564 = AXIS2_PLACEMENT_3D ( 'NONE', #14105, #3204, #1666 ) ;
#565 = ADVANCED_FACE ( 'NONE', ( #2546 ), #3319, .F. ) ;
#566 = DIRECTION ( 'NONE',  ( 0.000000000000000000, 0.000000000000000000, 1.000000000000000000 ) ) ;
#567 = DIRECTION ( 'NONE',  ( 0.000000000000000000, 1.000000000000000000, 0.000000000000000000 ) ) ;
#568 = CARTESIAN_POINT ( 'NONE',  ( -0.1669561253487713837, -0.4569961989594632512, 0.2467937633337932146 ) ) ;
#569 = DIRECTION ( 'NONE',  ( -7.017815000000000124E-18, 1.000000000000000000, -1.224646799147353207E-16 ) ) ;
#570 = CARTESIAN_POINT ( 'NONE',  ( 0.3105958729527036888, -0.6467467715322953170, 0.3122824329341910010 ) ) ;
#571 = AXIS2_PLACEMENT_3D ( 'NONE', #26308, #7804, #10047 ) ;
#572 = CARTESIAN_POINT ( 'NONE',  ( 0.04957542349328453862, 0.06229891813554931657, -0.4653527282821430799 ) ) ;
#573 = FACE_BOUND ( 'NONE', #23313, .T. ) ;
#574 = CARTESIAN_POINT ( 'NONE',  ( -0.2904160862623708650, 0.1677079028045392328, 1.953740157480315043 ) ) ;
#575 = B_SPLINE_CURVE_WITH_KNOTS ( 'NONE', 3,
 ( #21559, #25522, #19016, #21142, #6187, #25800, #4193, #19296, #10823, #27882 ),
 .UNSPECIFIED., .F., .F.,
 ( 4, 2, 2, 2, 4 ),
 ( 0.000000000000000000, 0.2500000000000000000, 0.5000000000000000000, 0.7500000000000000000, 1.000000000000000000 ),
 .UNSPECIFIED. ) ;
#576 = ORIENTED_EDGE ( 'NONE', *, *, #1922, .T. ) ;
#577 = CARTESIAN_POINT ( 'NONE',  ( 0.000000000000000000, 0.000000000000000000, 0.2362204724409449064 ) ) ;
#578 = EDGE_CURVE ( 'NONE', #17699, #24360, #11458, .T. ) ;
#579 = CARTESIAN_POINT ( 'NONE',  ( -0.5131133041954075713, -0.2529800193559338384, 0.9399606299212598381 ) ) ;
#580 = ADVANCED_FACE ( 'NONE', ( #26282 ), #25912, .F. ) ;
#581 = CARTESIAN_POINT ( 'NONE',  ( -0.2577577458591217563, -0.4472135058506044314, 1.766732283464566899 ) ) ;
#582 = CARTESIAN_POINT ( 'NONE',  ( -0.1291602287245499914, -0.3543605079199910191, 0.07637549214372835182 ) ) ;
#584 = DIRECTION ( 'NONE',  ( 0.000000000000000000, 0.000000000000000000, 1.000000000000000000 ) ) ;
#585 = EDGE_CURVE ( 'NONE', #20760, #20801, #19125, .T. ) ;
#586 = CIRCLE ( 'NONE', #13192, 0.3464566929133857665 ) ;
#587 = CIRCLE ( 'NONE', #3254, 0.8267716535433071723 ) ;
#588 = EDGE_CURVE ( 'NONE', #1674, #11878, #12352, .T. ) ;
#589 = ORIENTED_EDGE ( 'NONE', *, *, #19290, .F. ) ;
#590 = DIRECTION ( 'NONE',  ( -1.000000000000000000, 1.224646799147346305E-16, 0.000000000000000000 ) ) ;
#591 = DIRECTION ( 'NONE',  ( 0.000000000000000000, 0.000000000000000000, 1.000000000000000000 ) ) ;
#592 = ORIENTED_EDGE ( 'NONE', *, *, #21913, .F. ) ;
#593 = CARTESIAN_POINT ( 'NONE',  ( 0.2019525613798653918, -0.3664466487725785426, 0.6347042139374529102 ) ) ;
#594 = ORIENTED_EDGE ( 'NONE', *, *, #26108, .T. ) ;
#595 = ADVANCED_FACE ( 'NONE', ( #719 ), #17319, .T. ) ;
#596 = B_SPLINE_CURVE_WITH_KNOTS ( 'NONE', 3,
 ( #25551, #6069, #1950, #3792, #12413, #10279 ),
 .UNSPECIFIED., .F., .F.,
 ( 4, 2, 4 ),
 ( 0.6902184472752670441, 0.6915327610580710438, 0.6928470748408740443 ),
 .UNSPECIFIED. ) ;
#597 = CARTESIAN_POINT ( 'NONE',  ( -1.928513779527558736E-17, 0.000000000000000000, -0.4448818897637791814 ) ) ;
#598 = CARTESIAN_POINT ( 'NONE',  ( 0.6996455634117477729, -0.1588938903152396498, 0.3122824329354899064 ) ) ;
#599 = CARTESIAN_POINT ( 'NONE',  ( 0.7872492035923605025, 0.2530564255242896410, -0.2780832379081621952 ) ) ;
#600 = CIRCLE ( 'NONE', #12333, 0.8267716535433071723 ) ;
#601 = CARTESIAN_POINT ( 'NONE',  ( -0.06048688188729484105, 0.2165354330708661734, -3.626935712834467029 ) ) ;
#602 = CARTESIAN_POINT ( 'NONE',  ( 0.000000000000000000, 0.000000000000000000, 0.2637795275590551491 ) ) ;
#603 = ORIENTED_EDGE ( 'NONE', *, *, #16550, .T. ) ;
#604 = CARTESIAN_POINT ( 'NONE',  ( -0.4302903874076512425, -0.2491168502841591137, 0.1615162260931827798 ) ) ;
#605 = CARTESIAN_POINT ( 'NONE',  ( 0.1275996891957845991, -0.4763861460130774939, -1.550196850393700920 ) ) ;
#606 = CARTESIAN_POINT ( 'NONE',  ( 0.03001016326913514068, -0.4585215200179055817, -1.928289503579156516 ) ) ;
#607 = VERTEX_POINT ( 'NONE', #866 ) ;
#608 = EDGE_CURVE ( 'NONE', #21708, #2190, #18099, .T. ) ;
#609 = B_SPLINE_CURVE_WITH_KNOTS ( 'NONE', 3,
 ( #16712, #27310, #3855, #5987 ),
 .UNSPECIFIED., .F., .F.,
 ( 4, 4 ),
 ( 0.000000000000000000, 1.000000000000000000 ),
 .UNSPECIFIED. ) ;
#610 = CARTESIAN_POINT ( 'NONE',  ( 0.0005114926878545973925, 0.3662580330867914458, 0.1910323753037862504 ) ) ;
#611 = AXIS2_PLACEMENT_3D ( 'NONE', #25131, #20899, #5796 ) ;
#612 = CARTESIAN_POINT ( 'NONE',  ( 0.07874015748238459567, -0.03414999754297557560, -0.4724409448841456749 ) ) ;
#613 = CARTESIAN_POINT ( 'NONE',  ( 0.3714952424334504455, 0.06515381386493819538, 0.1992142436757342316 ) ) ;
#614 = APPLICATION_CONTEXT ( 'automotive_design' ) ;
#615 = EDGE_CURVE ( 'NONE', #12438, #5795, #14823, .T. ) ;
#616 = DIRECTION ( 'NONE',  ( 0.000000000000000000, 0.000000000000000000, 1.000000000000000000 ) ) ;
#617 = EDGE_CURVE ( 'NONE', #8913, #147, #1095, .T. ) ;
#618 = CARTESIAN_POINT ( 'NONE',  ( -0.0005057506112066828281, 0.6881888373222776467, 0.3401591245381555551 ) ) ;
#619 = CARTESIAN_POINT ( 'NONE',  ( 0.2988215684304370012, -0.6199272547993012195, 0.3401599409343967761 ) ) ;
#620 = DIRECTION ( 'NONE',  ( -1.000000000000000000, 0.000000000000000000, 0.000000000000000000 ) ) ;
#621 = CARTESIAN_POINT ( 'NONE',  ( -0.5383572925356228112, -0.3100567972183445042, 0.2574803149606298969 ) ) ;
#622 = CLOSED_SHELL ( 'NONE', ( #8560, #18644, #16249, #1256, #26576, #22771, #9012, #3173 ) ) ;
#623 = CARTESIAN_POINT ( 'NONE',  ( 0.000000000000000000, 0.000000000000000000, -0.05511811023622047168 ) ) ;
#624 = CARTESIAN_POINT ( 'NONE',  ( -0.6020308615105518513, -0.5839868939189144514, 0.9562171551411200454 ) ) ;
#625 = FACE_OUTER_BOUND ( 'NONE', #9890, .T. ) ;
#626 = DIRECTION ( 'NONE',  ( 0.000000000000000000, 1.000000000000000000, 0.000000000000000000 ) ) ;
#627 = EDGE_LOOP ( 'NONE', ( #9029, #26205 ) ) ;
#628 = CARTESIAN_POINT ( 'NONE',  ( -0.6633461167951516524, 0.02279600110638677068, 0.07858347093486456325 ) ) ;
#629 = ORIENTED_EDGE ( 'NONE', *, *, #18848, .T. ) ;
#630 = TOROIDAL_SURFACE ( 'NONE', #15950, 0.3198827364362346048, 0.01377952755905511792 ) ;
#631 = PLANE ( 'NONE',  #22046 ) ;
#632 = DIRECTION ( 'NONE',  ( 1.000000000000000000, 0.000000000000000000, 0.000000000000000000 ) ) ;
#633 = AXIS2_PLACEMENT_3D ( 'NONE', #14574, #25279, #27129 ) ;
#634 = CARTESIAN_POINT ( 'NONE',  ( 0.3665264996331779601, -0.2116141732283464416, 0.2145688976377952695 ) ) ;
#635 = ADVANCED_FACE ( 'NONE', ( #22183 ), #9450, .T. ) ;
#636 = CARTESIAN_POINT ( 'NONE',  ( -0.2227458012934312725, -0.3858827008515844370, -1.934055118110236560 ) ) ;
#637 = CARTESIAN_POINT ( 'NONE',  ( -0.3384212623783161011, 0.1668516812751324463, -3.100567304031758287 ) ) ;
#638 = DIRECTION ( 'NONE',  ( -1.000000000000000000, 0.000000000000000000, 0.000000000000000000 ) ) ;
#639 = DIRECTION ( 'NONE',  ( 0.000000000000000000, 0.000000000000000000, 1.000000000000000000 ) ) ;
#640 = ORIENTED_EDGE ( 'NONE', *, *, #8614, .T. ) ;
#641 = CARTESIAN_POINT ( 'NONE',  ( -0.2478439864030018425, -0.4300129863948121134, -1.569881889763780070 ) ) ;
#642 = APPLICATION_PROTOCOL_DEFINITION ( 'draft international standard', 'automotive_design', 1998, #5484 ) ;
#643 = AXIS2_PLACEMENT_3D ( 'NONE', #12530, #2842, #19821 ) ;
#644 = ORIENTED_EDGE ( 'NONE', *, *, #7697, .T. ) ;
#645 = AXIS2_PLACEMENT_3D ( 'NONE', #18436, #14238, #22419 ) ;
#646 = EDGE_LOOP ( 'NONE', ( #20143, #20285, #18872, #16802, #20608, #22874 ) ) ;
#647 = LINE ( 'NONE', #6869, #25949 ) ;
#648 = CARTESIAN_POINT ( 'NONE',  ( -0.01968503937007897581, 0.8214970631411201429, 1.006043748884723849E-16 ) ) ;
#649 = CARTESIAN_POINT ( 'NONE',  ( -0.1327036767659477978, -0.4954415918530775120, 1.747047244094488194 ) ) ;
#650 = ( CONVERSION_BASED_UNIT ( 'INCH', #22538 ) LENGTH_UNIT ( ) NAMED_UNIT ( #5813 ) ) ;
#651 = CARTESIAN_POINT ( 'NONE',  ( 0.2962590301041581609, -0.2272836761397895311, -3.115157480314960647 ) ) ;
#652 = CYLINDRICAL_SURFACE ( 'NONE', #15066, 0.2952755905264887182 ) ;
#653 = DIRECTION ( 'NONE',  ( 0.000000000000000000, -1.000000000000000000, 0.000000000000000000 ) ) ;
#654 = VECTOR ( 'NONE', #25570, 39.37007874015748143 ) ;
#655 = ORIENTED_EDGE ( 'NONE', *, *, #26490, .T. ) ;
#656 = CARTESIAN_POINT ( 'NONE',  ( 0.1677079028045289355, -0.2904160862623609840, 1.953740157480315043 ) ) ;
#657 = VERTEX_POINT ( 'NONE', #15970 ) ;
#658 = ORIENTED_EDGE ( 'NONE', *, *, #21103, .T. ) ;
#659 = CARTESIAN_POINT ( 'NONE',  ( 0.6119360453657125554, 0.1072290460171897442, 0.09685039370078740717 ) ) ;
#660 = ORIENTED_EDGE ( 'NONE', *, *, #22423, .T. ) ;
#661 = VERTEX_POINT ( 'NONE', #24573 ) ;
#662 = ORIENTED_EDGE ( 'NONE', *, *, #19173, .T. ) ;
#663 = ADVANCED_FACE ( 'NONE', ( #5225 ), #20348, .T. ) ;
#664 = DIRECTION ( 'NONE',  ( 0.000000000000000000, 0.000000000000000000, 1.000000000000000000 ) ) ;
#665 = EDGE_CURVE ( 'NONE', #15651, #12947, #18212, .T. ) ;
#666 = EDGE_CURVE ( 'NONE', #8687, #1454, #4948, .T. ) ;
#667 = VECTOR ( 'NONE', #27557, 39.37007874015748143 ) ;
#668 = FACE_OUTER_BOUND ( 'NONE', #21089, .T. ) ;
#669 = PRODUCT_DEFINITION ( 'UNKNOWN', '', #23773, #14490 ) ;
#670 = AXIS2_PLACEMENT_3D ( 'NONE', #15079, #14812, #19294 ) ;
#671 = DIRECTION ( 'NONE',  ( 0.000000000000000000, -1.000000000000000000, 0.000000000000000000 ) ) ;
#672 = CARTESIAN_POINT ( 'NONE',  ( 0.6932508136109228891, 0.7757875710709564165, -0.02341522039927820473 ) ) ;
#673 = ADVANCED_FACE ( 'NONE', ( #14428 ), #18626, .T. ) ;
#674 = CARTESIAN_POINT ( 'NONE',  ( 0.04956879728060029772, 0.2165354330708661457, -3.186635197996628310 ) ) ;
#675 = EDGE_CURVE ( 'NONE', #10287, #12118, #11029, .T. ) ;
#676 = EDGE_CURVE ( 'NONE', #25669, #5138, #6693, .T. ) ;
#677 = AXIS2_PLACEMENT_3D ( 'NONE', #5334, #26801, #20450 ) ;
#678 = DIRECTION ( 'NONE',  ( 0.000000000000000000, 0.000000000000000000, 1.000000000000000000 ) ) ;
#679 = CARTESIAN_POINT ( 'NONE',  ( 0.1512834625131836974, 0.2028719039650156708, -0.4452748529150018508 ) ) ;
#680 = CARTESIAN_POINT ( 'NONE',  ( -0.1968503937007874127, -0.07874015748031495954, -0.04546065111729331171 ) ) ;
#681 = CARTESIAN_POINT ( 'NONE',  ( 0.07874015748238459567, -0.03414999754297557560, -0.4724409448841456749 ) ) ;
#682 = SPHERICAL_SURFACE ( 'NONE', #15113, 0.1299232283464566984 ) ;
#683 = CARTESIAN_POINT ( 'NONE',  ( 0.1649135259617122706, 0.4856708409200614640, 1.766732283464566899 ) ) ;
#684 = AXIS2_PLACEMENT_3D ( 'NONE', #21009, #24675, #18877 ) ;
#685 = DIRECTION ( 'NONE',  ( 0.000000000000000000, 0.000000000000000000, 1.000000000000000000 ) ) ;
#686 = ORIENTED_EDGE ( 'NONE', *, *, #11935, .F. ) ;
#687 = AXIS2_PLACEMENT_3D ( 'NONE', #19653, #20189, #4936 ) ;
#688 = FACE_OUTER_BOUND ( 'NONE', #8896, .T. ) ;
#689 = LENGTH_MEASURE_WITH_UNIT ( LENGTH_MEASURE( 0.02539999999999999897 ), #14996 ) ;
#690 = ORIENTED_EDGE ( 'NONE', *, *, #10619, .F. ) ;
#691 = CARTESIAN_POINT ( 'NONE',  ( -0.3667122560601319692, 0.09855118063547732565, -3.100567304031763616 ) ) ;
#692 = ORIENTED_EDGE ( 'NONE', *, *, #26206, .T. ) ;
#693 = CARTESIAN_POINT ( 'NONE',  ( 0.000000000000000000, 0.000000000000000000, 0.3425196850393700809 ) ) ;
#694 = DIRECTION ( 'NONE',  ( -0.000000000000000000, -1.000000000000000000, -0.000000000000000000 ) ) ;
#695 = ORIENTED_EDGE ( 'NONE', *, *, #25428, .F. ) ;
#696 = CARTESIAN_POINT ( 'NONE',  ( 0.5131133041954023533, 0.2529800193559384458, 0.9399606299212598381 ) ) ;
#697 = ORIENTED_EDGE ( 'NONE', *, *, #23351, .F. ) ;
#698 = CIRCLE ( 'NONE', #4312, 0.5570866141732283561 ) ;
#699 = CARTESIAN_POINT ( 'NONE',  ( 0.3759206409296169116, 0.2989751379763687655, 0.2362204724409450174 ) ) ;
#700 = DIRECTION ( 'NONE',  ( 0.000000000000000000, -1.000000000000000000, 0.000000000000000000 ) ) ;
#701 = EDGE_CURVE ( 'NONE', #51, #18891, #12838, .T. ) ;
#702 = CARTESIAN_POINT ( 'NONE',  ( -0.0005939837304750000086, 0.5007870493127504208, 0.2574803149606298969 ) ) ;
#703 = CARTESIAN_POINT ( 'NONE',  ( 0.03532354024591842501, -0.6299212598425196763, 0.000000000000000000 ) ) ;
#704 = CARTESIAN_POINT ( 'NONE',  ( 0.09842519685039355370, 0.2165354330708661457, -3.548228346456693050 ) ) ;
#705 = EDGE_CURVE ( 'NONE', #13715, #9472, #19846, .T. ) ;
#706 = DIRECTION ( 'NONE',  ( -0.000000000000000000, -1.000000000000000000, -0.000000000000000000 ) ) ;
#707 = DIRECTION ( 'NONE',  ( 1.000000000000000000, 0.000000000000000000, 0.000000000000000000 ) ) ;
#708 = FACE_OUTER_BOUND ( 'NONE', #15095, .T. ) ;
#709 = EDGE_CURVE ( 'NONE', #4045, #152, #22753, .T. ) ;
#710 = AXIS2_PLACEMENT_3D ( 'NONE', #24848, #16245, #9579 ) ;
#711 = CARTESIAN_POINT ( 'NONE',  ( 0.2521176338356516666, -0.2211428102655709216, 1.953740157480315043 ) ) ;
#712 = DIRECTION ( 'NONE',  ( 0.000000000000000000, -1.000000000000000000, 0.000000000000000000 ) ) ;
#713 = SHAPE_REPRESENTATION ( 'Cam Shaft', ( #11588 ), #2999 ) ;
#714 = DIRECTION ( 'NONE',  ( -0.9575713608335526539, 0.1440981340193007720, -0.2495852893972995146 ) ) ;
#715 = DIRECTION ( 'NONE',  ( 0.4999999999999998890, -0.8660254037844388186, 0.000000000000000000 ) ) ;
#716 = AXIS2_PLACEMENT_3D ( 'NONE', #13335, #23940, #21541 ) ;
#717 = CARTESIAN_POINT ( 'NONE',  ( -0.6562077975700453258, 2.612916929133858441E-14, 0.2362204724409449064 ) ) ;
#718 = CARTESIAN_POINT ( 'NONE',  ( 0.4984899526255158753, -0.1339654526248288402, 1.766732283464567788 ) ) ;
#719 = FACE_OUTER_BOUND ( 'NONE', #2456, .T. ) ;
#720 = VERTEX_POINT ( 'NONE', #7488 ) ;
#721 = CARTESIAN_POINT ( 'NONE',  ( 0.006151574803149606648, 0.000000000000000000, 0.000000000000000000 ) ) ;
#722 = VECTOR ( 'NONE', #23360, 39.37007874015748854 ) ;
#723 = EDGE_CURVE ( 'NONE', #11887, #24760, #20053, .T. ) ;
#724 = VERTEX_POINT ( 'NONE', #23035 ) ;
#725 = ORIENTED_EDGE ( 'NONE', *, *, #8155, .T. ) ;
#726 = DIRECTION ( 'NONE',  ( 0.000000000000000000, 0.000000000000000000, -1.000000000000000000 ) ) ;
#727 = AXIS2_PLACEMENT_3D ( 'NONE', #14437, #3821, #3372 ) ;
#728 = CARTESIAN_POINT ( 'NONE',  ( 0.5385210225480960844, 0.4284847435812472183, 0.1322834645669291320 ) ) ;
#729 = DIRECTION ( 'NONE',  ( 0.000000000000000000, 1.000000000000000000, 0.000000000000000000 ) ) ;
#730 = VERTEX_POINT ( 'NONE', #18485 ) ;
#731 = DIRECTION ( 'NONE',  ( 0.000000000000000000, 1.000000000000000000, 0.000000000000000000 ) ) ;
#732 = ORIENTED_EDGE ( 'NONE', *, *, #14585, .T. ) ;
#733 = ADVANCED_FACE ( 'NONE', ( #27132 ), #5805, .T. ) ;
#734 = DIRECTION ( 'NONE',  ( -0.000000000000000000, 1.000000000000000000, 0.000000000000000000 ) ) ;
#735 = CARTESIAN_POINT ( 'NONE',  ( 0.1447526197146039584, -0.3977045540727763839, 0.2145688976377952695 ) ) ;
#736 = CARTESIAN_POINT ( 'NONE',  ( 0.7845931698711713365, 0.4599168999537228686, -0.01300178342961078731 ) ) ;
#737 = ADVANCED_FACE ( 'NONE', ( #1144 ), #9744, .T. ) ;
#738 = CARTESIAN_POINT ( 'NONE',  ( 0.3765118517642104257, -2.263258471485603576E-17, -3.100567304031763172 ) ) ;
#739 = CARTESIAN_POINT ( 'NONE',  ( 0.000000000000000000, 0.000000000000000000, -1.092739370078740131E-17 ) ) ;
#740 = ORIENTED_EDGE ( 'NONE', *, *, #20229, .T. ) ;
#741 = CARTESIAN_POINT ( 'NONE',  ( 0.3007905576423847704, 0.1482986320106501610, 1.973425196850393970 ) ) ;
#742 = CARTESIAN_POINT ( 'NONE',  ( -0.5118110236220182463, 0.03349795313034509281, -1.550196850393700920 ) ) ;
#743 = CARTESIAN_POINT ( 'NONE',  ( -0.2297883689023225706, -0.3979194638820617858, -1.928289503579150077 ) ) ;
#744 = AXIS2_PLACEMENT_3D ( 'NONE', #23603, #8466, #25702 ) ;
#745 = LINE ( 'NONE', #11474, #16 ) ;
#746 = EDGE_CURVE ( 'NONE', #25825, #26393, #21042, .T. ) ;
#747 = CARTESIAN_POINT ( 'NONE',  ( 0.6117833106356003192, 0.1080972763116094665, 0.2574827755769819038 ) ) ;
#748 = CARTESIAN_POINT ( 'NONE',  ( 0.1638952246732497953, 0.5499255957412874096, 0.000000000000000000 ) ) ;
#749 = DIRECTION ( 'NONE',  ( 0.000000000000000000, 0.000000000000000000, -1.000000000000000000 ) ) ;
#750 = CARTESIAN_POINT ( 'NONE',  ( 0.1188866373884869265, 0.4438564651657460614, -1.928289503579154740 ) ) ;
#751 = EDGE_CURVE ( 'NONE', #9997, #27369, #23688, .T. ) ;
#752 = CARTESIAN_POINT ( 'NONE',  ( -0.03220957031754000111, 0.4921259842519685179, -1.569881889763779625 ) ) ;
#753 = TOROIDAL_SURFACE ( 'NONE', #16532, 0.7165354330708662012, 0.01181102362204724393 ) ;
#754 = CARTESIAN_POINT ( 'NONE',  ( -0.1259131187103122163, 1.099024551511217362, -0.3668305760060864840 ) ) ;
#755 = DIRECTION ( 'NONE',  ( -0.000000000000000000, -1.000000000000000000, -0.000000000000000000 ) ) ;
#756 = CARTESIAN_POINT ( 'NONE',  ( 0.4724409448465559103, 5.785732908924860203E-17, 1.953740157480315043 ) ) ;
#757 = DIRECTION ( 'NONE',  ( 0.000000000000000000, 0.000000000000000000, 1.000000000000000000 ) ) ;
#758 = FACE_BOUND ( 'NONE', #21251, .T. ) ;
#759 = PLANE ( 'NONE',  #24631 ) ;
#760 = B_SPLINE_CURVE_WITH_KNOTS ( 'NONE', 3,
 ( #11709, #11429, #14120, #13834, #3353, #22726 ),
 .UNSPECIFIED., .F., .F.,
 ( 4, 2, 4 ),
 ( 0.9031406754215589583, 0.9046454396443730506, 0.9061502038671870318 ),
 .UNSPECIFIED. ) ;
#761 = CARTESIAN_POINT ( 'NONE',  ( -7.608238775805210269E-17, -0.6212598425196850238, 0.3059055118110236560 ) ) ;
#762 = VERTEX_POINT ( 'NONE', #16114 ) ;
#763 = CARTESIAN_POINT ( 'NONE',  ( -0.1775236553381950300, 0.3075341118176279642, 1.953740157480315487 ) ) ;
#764 = VERTEX_POINT ( 'NONE', #8065 ) ;
#765 = EDGE_CURVE ( 'NONE', #26553, #20265, #18689, .T. ) ;
#766 = CARTESIAN_POINT ( 'NONE',  ( 0.4498374011142918794, -0.05926487674658236643, -1.934055118110236338 ) ) ;
#767 = EDGE_CURVE ( 'NONE', #19729, #5602, #7540, .T. ) ;
#768 = CARTESIAN_POINT ( 'NONE',  ( 0.0006679551606482677165, 0.5322830454629158270, 0.3401574803149606252 ) ) ;
#769 = CARTESIAN_POINT ( 'NONE',  ( -0.4931105264837953306, 0.08735026989778622852, 0.09684874903502814492 ) ) ;
#770 = FACE_OUTER_BOUND ( 'NONE', #2926, .T. ) ;
#771 = AXIS2_PLACEMENT_3D ( 'NONE', #1458, #21348, #1986 ) ;
#772 = CARTESIAN_POINT ( 'NONE',  ( 0.000000000000000000, 0.000000000000000000, 0.3425196850393700809 ) ) ;
#773 = CARTESIAN_POINT ( 'NONE',  ( 0.1493402947442837025, 0.2231667116155127972, 0.4250100353273641440 ) ) ;
#774 = LINE ( 'NONE', #17967, #26208 ) ;
#775 = EDGE_CURVE ( 'NONE', #24094, #88, #25559, .T. ) ;
#776 = DIRECTION ( 'NONE',  ( 0.000000000000000000, 0.000000000000000000, 1.000000000000000000 ) ) ;
#777 = MECHANICAL_DESIGN_GEOMETRIC_PRESENTATION_REPRESENTATION (  '', ( #15229 ), #16556 ) ;
#778 = CARTESIAN_POINT ( 'NONE',  ( -0.4446020952038909901, -0.02920026389085020324, -1.934055118110237448 ) ) ;
#779 = CARTESIAN_POINT ( 'NONE',  ( -0.1668516812751421607, 0.3384212623783116602, -3.100567304031759175 ) ) ;
#780 = ( REPRESENTATION_RELATIONSHIP ('NONE','NONE', #12434, #9188 ) REPRESENTATION_RELATIONSHIP_WITH_TRANSFORMATION ( #15247 )SHAPE_REPRESENTATION_RELATIONSHIP( ) ) ;
#781 = DIRECTION ( 'NONE',  ( 0.000000000000000000, -0.8660254037844389297, -0.4999999999999994449 ) ) ;
#782 = CYLINDRICAL_SURFACE ( 'NONE', #20278, 0.4330708661417322913 ) ;
#783 = VERTEX_POINT ( 'NONE', #2370 ) ;
#784 = CARTESIAN_POINT ( 'NONE',  ( -0.3858397471888794783, 0.2228126397720086582, -1.934055118110236338 ) ) ;
#785 = ORIENTED_EDGE ( 'NONE', *, *, #9722, .F. ) ;
#786 = ORIENTED_EDGE ( 'NONE', *, *, #1340, .T. ) ;
#787 = AXIS2_PLACEMENT_3D ( 'NONE', #1589, #5844, #3272 ) ;
#788 = AXIS2_PLACEMENT_3D ( 'NONE', #5285, #22529, #17715 ) ;
#789 = ORIENTED_EDGE ( 'NONE', *, *, #20752, .F. ) ;
#790 = FACE_OUTER_BOUND ( 'NONE', #25634, .T. ) ;
#791 = FACE_OUTER_BOUND ( 'NONE', #25595, .T. ) ;
#792 = CARTESIAN_POINT ( 'NONE',  ( 0.2564944395515950104, 0.4441657790108120563, 1.747047244094488194 ) ) ;
#793 = ORIENTED_EDGE ( 'NONE', *, *, #18272, .F. ) ;
#794 = CARTESIAN_POINT ( 'NONE',  ( 0.3702005978258383068, -0.04877294052296102245, -3.115157480314960647 ) ) ;
#795 = EDGE_LOOP ( 'NONE', ( #9740, #5198 ) ) ;
#796 = CARTESIAN_POINT ( 'NONE',  ( 0.7874015748031496509, 0.2841772834048059693, -0.1654443243217737780 ) ) ;
#797 = CARTESIAN_POINT ( 'NONE',  ( -1.928513779527558736E-17, 0.000000000000000000, -0.03543307086614204404 ) ) ;
#798 = VERTEX_POINT ( 'NONE', #6495 ) ;
#799 = ORIENTED_EDGE ( 'NONE', *, *, #16948, .T. ) ;
#800 = ORIENTED_EDGE ( 'NONE', *, *, #13640, .T. ) ;
#801 = ORIENTED_EDGE ( 'NONE', *, *, #20824, .F. ) ;
#802 = CARTESIAN_POINT ( 'NONE',  ( 0.1152775731717068236, 0.4303822302054135518, -1.934055118110236338 ) ) ;
#803 = ORIENTED_EDGE ( 'NONE', *, *, #20955, .T. ) ;
#804 = VERTEX_POINT ( 'NONE', #4097 ) ;
#805 = CARTESIAN_POINT ( 'NONE',  ( -0.6912180915490531152, 0.1281909420063060967, 0.2299950541617507838 ) ) ;
#806 = CARTESIAN_POINT ( 'NONE',  ( -0.2952755905264887182, 3.616083068046089993E-17, -4.330708661417323135 ) ) ;
#807 = EDGE_CURVE ( 'NONE', #21046, #2655, #23735, .T. ) ;
#808 = CIRCLE ( 'NONE', #5781, 0.003937007874015741038 ) ;
#809 = PLANE ( 'NONE',  #6198 ) ;
#810 = ( GEOMETRIC_REPRESENTATION_CONTEXT ( 3 ) GLOBAL_UNCERTAINTY_ASSIGNED_CONTEXT ( ( #7702 ) ) GLOBAL_UNIT_ASSIGNED_CONTEXT ( ( #15259, #9007, #8602 ) ) REPRESENTATION_CONTEXT ( 'NONE', 'WORKASPACE' ) ) ;
#811 = DIRECTION ( 'NONE',  ( 0.000000000000000000, 1.000000000000000000, 0.000000000000000000 ) ) ;
#812 = DIRECTION ( 'NONE',  ( 1.000000000000000000, 0.000000000000000000, 0.000000000000000000 ) ) ;
#813 = DIRECTION ( 'NONE',  ( 1.000000000000000000, 0.000000000000000000, 0.000000000000000000 ) ) ;
#814 = PRODUCT_DEFINITION_SHAPE ( 'NONE', 'NONE',  #27911 ) ;
#815 = DIRECTION ( 'NONE',  ( 1.000000000000000000, 0.000000000000000000, 0.000000000000000000 ) ) ;
#816 = CARTESIAN_POINT ( 'NONE',  ( -0.04380501567505455662, -0.3346456692913385433, 1.973425196850393970 ) ) ;
#817 = CARTESIAN_POINT ( 'NONE',  ( 0.3184841198566381593, 0.1570220809524529026, 1.953740157480315043 ) ) ;
#818 = CARTESIAN_POINT ( 'NONE',  ( 0.6117062799105531523, 0.1085321106658064944, 0.2574803149606298969 ) ) ;
#819 = CARTESIAN_POINT ( 'NONE',  ( -0.2303471512294322787, -0.4798602677570401598, 0.1322834645669291320 ) ) ;
#820 = DIRECTION ( 'NONE',  ( -0.9848077530122079093, 0.1736481776669309696, 0.000000000000000000 ) ) ;
#821 = DIRECTION ( 'NONE',  ( 0.000000000000000000, 0.000000000000000000, -1.000000000000000000 ) ) ;
#822 = CARTESIAN_POINT ( 'NONE',  ( -0.5280699926563170443, -0.06957181182498474448, 1.747047244094488194 ) ) ;
#823 = CARTESIAN_POINT ( 'NONE',  ( 0.5118110236220472231, 0.000000000000000000, 1.766732283464566899 ) ) ;
#824 = VECTOR ( 'NONE', #13835, 39.37007874015748143 ) ;
#825 = EDGE_CURVE ( 'NONE', #24109, #24279, #17361, .T. ) ;
#826 = CIRCLE ( 'NONE', #11202, 0.1298643763538141760 ) ;
#827 = ( BOUNDED_CURVE ( )  B_SPLINE_CURVE ( 2, ( #24895, #10448, #19350 ),
 .UNSPECIFIED., .F., .F. ) 
 B_SPLINE_CURVE_WITH_KNOTS ( ( 3, 3 ),
 ( 0.000000000000000000, 0.2336872276155829986 ),
 .UNSPECIFIED. ) 
 CURVE ( )  GEOMETRIC_REPRESENTATION_ITEM ( )  RATIONAL_B_SPLINE_CURVE ( ( 1.000000000000000000, 1.154700538379249908, 1.000000000000000000 ) ) 
 REPRESENTATION_ITEM ( '' )  ) ;
#828 = ORIENTED_EDGE ( 'NONE', *, *, #19338, .F. ) ;
#829 = CARTESIAN_POINT ( 'NONE',  ( 0.4121125639445893385, -0.2386018002037871011, 0.1212655228849990885 ) ) ;
#830 = VERTEX_POINT ( 'NONE', #16815 ) ;
#831 = TOROIDAL_SURFACE ( 'NONE', #22041, 0.3584231247409862542, 0.01377952755905511792 ) ;
#832 = CARTESIAN_POINT ( 'NONE',  ( 0.2118615749922464486, -0.5840192333899535404, 0.2574803149606298969 ) ) ;
#833 = VERTEX_POINT ( 'NONE', #19057 ) ;
#834 = CARTESIAN_POINT ( 'NONE',  ( -0.4065144339881236468, -0.2344790234878192936, 0.07637549214372835182 ) ) ;
#835 = ORIENTED_EDGE ( 'NONE', *, *, #3265, .T. ) ;
#836 = CARTESIAN_POINT ( 'NONE',  ( -0.4921259842519685179, -0.03220957031763953954, -1.569881889763779625 ) ) ;
#837 = CYLINDRICAL_SURFACE ( 'NONE', #12003, 0.1181102362204718703 ) ;
#838 = EDGE_CURVE ( 'NONE', #4142, #1699, #4370, .T. ) ;
#839 = ORIENTED_EDGE ( 'NONE', *, *, #24552, .T. ) ;
#840 = CARTESIAN_POINT ( 'NONE',  ( -0.4382482975804890546, -0.3362148458988509225, 0.9399606299212598381 ) ) ;
#841 = ORIENTED_EDGE ( 'NONE', *, *, #19527, .T. ) ;
#842 = CARTESIAN_POINT ( 'NONE',  ( 0.4092566936341573980, 0.3255244810069335970, 0.3331434174606269227 ) ) ;
#843 = DIRECTION ( 'NONE',  ( -0.9790454724845840673, 0.1018208755700876073, -0.1763589297585415050 ) ) ;
#844 = CIRCLE ( 'NONE', #25418, 0.1771653543307086798 ) ;
#845 = CARTESIAN_POINT ( 'NONE',  ( 0.000000000000000000, 0.3771653543307086909, 0.2755905511811023723 ) ) ;
#846 = B_SPLINE_CURVE_WITH_KNOTS ( 'NONE', 3,
 ( #20384, #22082, #9633, #24207 ),
 .UNSPECIFIED., .F., .F.,
 ( 4, 4 ),
 ( -1.254364830977226175, -0.8024850953550110022 ),
 .UNSPECIFIED. ) ;
#847 = CARTESIAN_POINT ( 'NONE',  ( -2.073220866141732523E-16, 0.4724409448818898127, 1.692913385826771533 ) ) ;
#848 = DIRECTION ( 'NONE',  ( 0.000000000000000000, 0.000000000000000000, 1.000000000000000000 ) ) ;
#849 = DIRECTION ( 'NONE',  ( -1.000000000000000000, 0.000000000000000000, 0.000000000000000000 ) ) ;
#850 = AXIS2_PLACEMENT_3D ( 'NONE', #25833, #6763, #15396 ) ;
#851 = AXIS2_PLACEMENT_3D ( 'NONE', #2037, #22857, #17156 ) ;
#852 = DIRECTION ( 'NONE',  ( 0.000000000000000000, 1.000000000000000000, 0.000000000000000000 ) ) ;
#853 = CARTESIAN_POINT ( 'NONE',  ( -0.3661417322834645272, -0.4724409448818898127, -0.8182917201112815953 ) ) ;
#854 = CARTESIAN_POINT ( 'NONE',  ( -0.1180276236025431108, -0.3257325899126714552, 0.1276989850612303967 ) ) ;
#855 = AXIS2_PLACEMENT_3D ( 'NONE', #18013, #5044, #5477 ) ;
#856 = CARTESIAN_POINT ( 'NONE',  ( -0.04380447413658625222, -0.3324885138898230341, 1.953740157480315043 ) ) ;
#857 = UNCERTAINTY_MEASURE_WITH_UNIT (LENGTH_MEASURE( 1.000000000000000082E-05 ), #18780, 'distance_accuracy_value', 'NONE') ;
#858 = VERTEX_POINT ( 'NONE', #2113 ) ;
#859 = PLANE ( 'NONE',  #25863 ) ;
#860 = CARTESIAN_POINT ( 'NONE',  ( 0.6106000000000000316, 0.09842519683305382683, 1.205361022570475770E-17 ) ) ;
#861 = DIRECTION ( 'NONE',  ( 1.000000000000000000, 1.000000000000000078E-15, 0.000000000000000000 ) ) ;
#862 = EDGE_CURVE ( 'NONE', #24185, #27369, #15261, .T. ) ;
#863 = CYLINDRICAL_SURFACE ( 'NONE', #6726, 0.7539370078740157410 ) ;
#864 = CARTESIAN_POINT ( 'NONE',  ( 0.2092582568863658732, -0.4359957531143022202, 0.2715646632236008440 ) ) ;
#865 = CIRCLE ( 'NONE', #10326, 0.1181102362204720091 ) ;
#866 = CARTESIAN_POINT ( 'NONE',  ( -0.7874015748031496509, 0.000000000000000000, -0.2362204724409448231 ) ) ;
#867 = CARTESIAN_POINT ( 'NONE',  ( 0.000000000000000000, 0.000000000000000000, 0.2362204724409449064 ) ) ;
#868 = EDGE_CURVE ( 'NONE', #18194, #14499, #21744, .T. ) ;
#869 = CARTESIAN_POINT ( 'NONE',  ( 0.06889763779527550980, 8.437527159479786693E-18, -0.2834645669291338543 ) ) ;
#870 = ORIENTED_EDGE ( 'NONE', *, *, #1826, .T. ) ;
#871 = EDGE_CURVE ( 'NONE', #12664, #8508, #14728, .T. ) ;
#872 = ORIENTED_EDGE ( 'NONE', *, *, #24132, .F. ) ;
#873 = AXIS2_PLACEMENT_3D ( 'NONE', #26941, #1100, #24946 ) ;
#874 = LINE ( 'NONE', #22052, #17827 ) ;
#875 = EDGE_CURVE ( 'NONE', #4894, #7494, #21145, .T. ) ;
#876 = DIRECTION ( 'NONE',  ( -0.8660254037844388186, 0.4999999999999998890, 0.000000000000000000 ) ) ;
#877 = AXIS2_PLACEMENT_3D ( 'NONE', #9629, #24334, #22215 ) ;
#878 = CARTESIAN_POINT ( 'NONE',  ( 0.09842519685039355370, 0.2165354330708661457, -3.548228346456692162 ) ) ;
#879 = ORIENTED_EDGE ( 'NONE', *, *, #17592, .T. ) ;
#880 = CARTESIAN_POINT ( 'NONE',  ( -0.09842519685039370636, 0.07874015748031495954, 0.04546065111729331171 ) ) ;
#881 = ORIENTED_EDGE ( 'NONE', *, *, #14494, .F. ) ;
#882 = CARTESIAN_POINT ( 'NONE',  ( -0.2255758929758618081, -0.6217623271429643106, 0.1616495878894404215 ) ) ;
#883 = AXIS2_PLACEMENT_3D ( 'NONE', #21381, #23084, #14476 ) ;
#884 = CARTESIAN_POINT ( 'NONE',  ( -0.3105951325225213000, -0.1787383246545907467, 0.09506557084360875431 ) ) ;
#885 = CARTESIAN_POINT ( 'NONE',  ( -2.685748425196850164E-17, 0.000000000000000000, -3.115157480314960647 ) ) ;
#886 = CARTESIAN_POINT ( 'NONE',  ( -0.3239425792934405024, 0.08676778863011171128, 1.973425196850393970 ) ) ;
#887 = CARTESIAN_POINT ( 'NONE',  ( -0.4931450244001936989, 0.08715529520342381320, 0.2574827755769819038 ) ) ;
#888 = CARTESIAN_POINT ( 'NONE',  ( 0.03220957031753916844, -0.4921259842519685179, -1.550196850393700920 ) ) ;
#889 = CIRCLE ( 'NONE', #13953, 0.08582677165167480748 ) ;
#890 = CARTESIAN_POINT ( 'NONE',  ( -0.3714653163189441387, 0.06532421472592696288, 0.07637549214372835182 ) ) ;
#891 = CARTESIAN_POINT ( 'NONE',  ( 0.5230301363771324707, 0.1775991818008611500, 0.9202755905511811330 ) ) ;
#892 = DIRECTION ( 'NONE',  ( 0.000000000000000000, -1.000000000000000000, 0.000000000000000000 ) ) ;
#893 = DIRECTION ( 'NONE',  ( 0.000000000000000000, 1.000000000000000000, 0.000000000000000000 ) ) ;
#894 = CIRCLE ( 'NONE', #26579, 0.1181102362204718703 ) ;
#895 = FACE_OUTER_BOUND ( 'NONE', #5397, .T. ) ;
#896 = CARTESIAN_POINT ( 'NONE',  ( 0.2031943647053748025, 0.4121342552748526455, -1.928289503579147190 ) ) ;
#897 = FACE_OUTER_BOUND ( 'NONE', #27032, .T. ) ;
#898 = DIRECTION ( 'NONE',  ( -0.9790454724845842893, -0.1018208755700884260, -0.1763589297585410332 ) ) ;
#899 = CARTESIAN_POINT ( 'NONE',  ( 0.2315507648392299000, -0.4792806379917101678, 0.1322834645669291320 ) ) ;
#900 = CARTESIAN_POINT ( 'NONE',  ( -0.3998447049182095037, 0.4754871227241110332, 0.2574803149606298969 ) ) ;
#901 = EDGE_CURVE ( 'NONE', #11142, #9968, #10681, .T. ) ;
#902 = CARTESIAN_POINT ( 'NONE',  ( 0.2307489990847578776, -0.4796672131996535526, 0.1322810039474933141 ) ) ;
#903 = ORIENTED_EDGE ( 'NONE', *, *, #16753, .T. ) ;
#904 = ( CONVERSION_BASED_UNIT ( 'INCH', #18242 ) LENGTH_UNIT ( ) NAMED_UNIT ( #24418 ) ) ;
#905 = CARTESIAN_POINT ( 'NONE',  ( -0.1771653543307086520, 0.5935039370078740717, 0.000000000000000000 ) ) ;
#906 = ORIENTED_EDGE ( 'NONE', *, *, #6294, .T. ) ;
#907 = CARTESIAN_POINT ( 'NONE',  ( 0.6299212598425196763, -0.4807043897637795493, 5.886930922602943265E-17 ) ) ;
#908 = ORIENTED_EDGE ( 'NONE', *, *, #10737, .T. ) ;
#909 = AXIS2_PLACEMENT_3D ( 'NONE', #18396, #16022, #13901 ) ;
#910 = CARTESIAN_POINT ( 'NONE',  ( 0.4157391792961063204, 0.3323952789219082882, 0.1322834645669291320 ) ) ;
#911 = EDGE_LOOP ( 'NONE', ( #11469, #21986 ) ) ;
#912 = DIRECTION ( 'NONE',  ( 1.000000000000000000, 0.000000000000000000, 0.000000000000000000 ) ) ;
#913 = FACE_OUTER_BOUND ( 'NONE', #10036, .T. ) ;
#914 = CARTESIAN_POINT ( 'NONE',  ( 0.08582765042225336261, 0.3030860912054640921, -3.222734230592224858 ) ) ;
#915 = CARTESIAN_POINT ( 'NONE',  ( 0.1755067523729419432, -0.3028750839302634112, 0.5245950337139047015 ) ) ;
#916 = DIRECTION ( 'NONE',  ( 0.000000000000000000, 0.000000000000000000, -1.000000000000000000 ) ) ;
#917 = CARTESIAN_POINT ( 'NONE',  ( 3.387491338582676985E-16, -0.6299212598425196763, 0.000000000000000000 ) ) ;
#918 = VECTOR ( 'NONE', #23051, 39.37007874015748143 ) ;
#919 = DIRECTION ( 'NONE',  ( 1.000000000000000000, 0.000000000000000000, 0.000000000000000000 ) ) ;
#920 = CARTESIAN_POINT ( 'NONE',  ( 0.3572819248074489140, -0.1213180142433802344, -3.100567304031756066 ) ) ;
#921 = DIRECTION ( 'NONE',  ( -1.000000000000000000, 0.000000000000000000, 0.000000000000000000 ) ) ;
#922 = ADVANCED_BREP_SHAPE_REPRESENTATION ( 'Cam Follower', ( #12666, #11588 ), #22004 ) ;
#923 = ORIENTED_EDGE ( 'NONE', *, *, #17887, .T. ) ;
#924 = DIRECTION ( 'NONE',  ( 1.000000000000000000, 0.000000000000000000, 0.000000000000000000 ) ) ;
#925 = CARTESIAN_POINT ( 'NONE',  ( -0.2228126397719833174, 0.3858397471888795893, -1.934055118110236338 ) ) ;
#926 = SHAPE_DEFINITION_REPRESENTATION ( #15254, #6338 ) ;
#927 = CARTESIAN_POINT ( 'NONE',  ( -0.7795729917428700917, 0.2877957735339043421, -0.2883818734248744242 ) ) ;
#928 = EDGE_CURVE ( 'NONE', #158, #23473, #6082, .T. ) ;
#929 = AXIS2_PLACEMENT_3D ( 'NONE', #24250, #9255, #13939 ) ;
#930 = ORIENTED_EDGE ( 'NONE', *, *, #14908, .T. ) ;
#931 = FACE_OUTER_BOUND ( 'NONE', #26813, .T. ) ;
#932 = CARTESIAN_POINT ( 'NONE',  ( 0.6751968503937006982, 8.353151887884997269E-17, -4.097771653543307347E-17 ) ) ;
#933 = CARTESIAN_POINT ( 'NONE',  ( 0.06699507805369034341, 0.5085118447801111330, 1.747047244094488194 ) ) ;
#934 = ADVANCED_FACE ( 'NONE', ( #12702 ), #12572, .T. ) ;
#935 = VERTEX_POINT ( 'NONE', #19202 ) ;
#936 = AXIS2_PLACEMENT_3D ( 'NONE', #3031, #24513, #15779 ) ;
#937 = CARTESIAN_POINT ( 'NONE',  ( -0.02464264302293797324, 0.3765118517642104257, -3.100567304031763172 ) ) ;
#938 = EDGE_LOOP ( 'NONE', ( #21430, #4636, #799, #17993 ) ) ;
#939 = CARTESIAN_POINT ( 'NONE',  ( -0.6299212598425196763, 1.087444635826771533, -0.1051828227901515783 ) ) ;
#940 = FACE_OUTER_BOUND ( 'NONE', #528, .T. ) ;
#941 = ORIENTED_EDGE ( 'NONE', *, *, #17711, .F. ) ;
#942 = ORIENTED_EDGE ( 'NONE', *, *, #7366, .T. ) ;
#943 = DIRECTION ( 'NONE',  ( 1.000000000000000000, 0.000000000000000000, 0.000000000000000000 ) ) ;
#944 = DIRECTION ( 'NONE',  ( -1.000000000000000000, 0.000000000000000000, 0.000000000000000000 ) ) ;
#945 = ORIENTED_EDGE ( 'NONE', *, *, #10724, .F. ) ;
#946 = EDGE_LOOP ( 'NONE', ( #5245, #370, #4472, #8238, #9152, #16696 ) ) ;
#947 = DIRECTION ( 'NONE',  ( 0.000000000000000000, 1.000000000000000000, 0.000000000000000000 ) ) ;
#948 = CARTESIAN_POINT ( 'NONE',  ( 0.07667729696052867638, 0.1968503937007874405, -3.568863587253130021 ) ) ;
#949 = EDGE_CURVE ( 'NONE', #26096, #20147, #2007, .T. ) ;
#950 = B_SPLINE_CURVE_WITH_KNOTS ( 'NONE', 2,
 ( #2095, #10422, #14562 ),
 .UNSPECIFIED., .F., .F.,
 ( 3, 3 ),
 ( 0.000000000000000000, 1.000000000000000000 ),
 .UNSPECIFIED. ) ;
#951 = VECTOR ( 'NONE', #3285, 39.37007874015748143 ) ;
#952 = CARTESIAN_POINT ( 'NONE',  ( -0.3392387706403475200, 0.1151913129404399938, -3.115157480314960647 ) ) ;
#953 = DIRECTION ( 'NONE',  ( 1.000000000000000000, 0.000000000000000000, 0.000000000000000000 ) ) ;
#954 = DIRECTION ( 'NONE',  ( 0.000000000000000000, 1.000000000000000000, 0.000000000000000000 ) ) ;
#955 = CARTESIAN_POINT ( 'NONE',  ( -0.3334645669291338987, 0.9667105296868090392, -0.8968761852611063512 ) ) ;
#956 = ( GEOMETRIC_REPRESENTATION_CONTEXT ( 3 ) GLOBAL_UNCERTAINTY_ASSIGNED_CONTEXT ( ( #13843 ) ) GLOBAL_UNIT_ASSIGNED_CONTEXT ( ( #21076, #968, #13392 ) ) REPRESENTATION_CONTEXT ( 'NONE', 'WORKASPACE' ) ) ;
#957 = CARTESIAN_POINT ( 'NONE',  ( 0.7871730179869350641, 0.2557924603611196890, -0.2773276354978094771 ) ) ;
#958 = CARTESIAN_POINT ( 'NONE',  ( 0.000000000000000000, 0.000000000000000000, -3.278217716535432842E-17 ) ) ;
#959 = CARTESIAN_POINT ( 'NONE',  ( -0.4062254136079196942, -0.2349793847445165174, 0.1992142434433712694 ) ) ;
#960 = CARTESIAN_POINT ( 'NONE',  ( -1.466875984251968630E-17, 0.000000000000000000, 0.000000000000000000 ) ) ;
#961 = CARTESIAN_POINT ( 'NONE',  ( -0.3543307086614173596, -0.02319089060378156514, 1.953740157480315043 ) ) ;
#962 = CARTESIAN_POINT ( 'NONE',  ( -0.7168072604740280962, -0.1644124225524362104, 0.2763636194370550636 ) ) ;
#963 = LINE ( 'NONE', #9553, #16645 ) ;
#964 = FACE_OUTER_BOUND ( 'NONE', #13122, .T. ) ;
#965 = DIRECTION ( 'NONE',  ( 0.000000000000000000, 0.000000000000000000, -1.000000000000000000 ) ) ;
#966 = CARTESIAN_POINT ( 'NONE',  ( -0.4004221243553304777, 0.3512268162760389667, 1.747047244094488194 ) ) ;
#967 = EDGE_CURVE ( 'NONE', #6542, #17886, #4274, .T. ) ;
#968 = ( NAMED_UNIT ( * ) PLANE_ANGLE_UNIT ( ) SI_UNIT ( $, .RADIAN. ) ) ;
#969 = EDGE_CURVE ( 'NONE', #16082, #26393, #16448, .T. ) ;
#970 = AXIS2_PLACEMENT_3D ( 'NONE', #18823, #8110, #11923 ) ;
#971 = CYLINDRICAL_SURFACE ( 'NONE', #8819, 0.8163976377952756325 ) ;
#972 = ORIENTED_EDGE ( 'NONE', *, *, #10601, .F. ) ;
#973 = CARTESIAN_POINT ( 'NONE',  ( 0.2243259791921815294, -0.6183223858027685482, 0.2081850588255441115 ) ) ;
#974 = CARTESIAN_POINT ( 'NONE',  ( -0.04632170870458265227, -0.3520570504767543962, 1.953740157480315043 ) ) ;
#975 = DIRECTION ( 'NONE',  ( 1.000000000000000000, 0.000000000000000000, 0.000000000000000000 ) ) ;
#976 = AXIS2_PLACEMENT_3D ( 'NONE', #6874, #2210, #8577 ) ;
#977 = ORIENTED_EDGE ( 'NONE', *, *, #2179, .T. ) ;
#978 = AXIS2_PLACEMENT_3D ( 'NONE', #24637, #18270, #11515 ) ;
#979 = CARTESIAN_POINT ( 'NONE',  ( 0.1585706980422492418, -0.4669911931914798586, -1.569881889763779625 ) ) ;
#980 = ORIENTED_EDGE ( 'NONE', *, *, #22815, .T. ) ;
#981 = CARTESIAN_POINT ( 'NONE',  ( -0.5671862884095143498, 0.07472527936311554320, 0.9399606299212598381 ) ) ;
#982 = ORIENTED_EDGE ( 'NONE', *, *, #7627, .T. ) ;
#983 = EDGE_LOOP ( 'NONE', ( #23970, #6463, #1289, #16251, #21520, #7050 ) ) ;
#984 = CARTESIAN_POINT ( 'NONE',  ( 0.5869493968219645641, 0.2133897621573078718, 0.3696019098714952711 ) ) ;
#985 = DIMENSIONAL_EXPONENTS ( 1.000000000000000000, 0.000000000000000000, 0.000000000000000000, 0.000000000000000000, 0.000000000000000000, 0.000000000000000000, 0.000000000000000000 ) ;
#986 = CARTESIAN_POINT ( 'NONE',  ( 0.2230788859036007821, 0.2650812153444456198, 0.1377952755905513527 ) ) ;
#987 = ITEM_DEFINED_TRANSFORMATION ( 'NONE', 'NONE', #16138,  #11588 ) ;
#988 = DIRECTION ( 'NONE',  ( 1.000000000000000000, 0.000000000000000000, 0.000000000000000000 ) ) ;
#989 = CARTESIAN_POINT ( 'NONE',  ( -0.3149606299212598381, 0.000000000000000000, 0.000000000000000000 ) ) ;
#990 = DIRECTION ( 'NONE',  ( 0.000000000000000000, 0.000000000000000000, -1.000000000000000000 ) ) ;
#991 = FACE_OUTER_BOUND ( 'NONE', #24406, .T. ) ;
#992 = EDGE_CURVE ( 'NONE', #13219, #8587, #11932, .T. ) ;
#993 = AXIS2_PLACEMENT_3D ( 'NONE', #65, #8764, #25589 ) ;
#994 = CARTESIAN_POINT ( 'NONE',  ( -0.1187185187216169419, -0.3276343780110584913, 0.1166443193947863527 ) ) ;
#995 = CARTESIAN_POINT ( 'NONE',  ( 0.3346456692913385988, 0.000000000000000000, 1.953740157480315043 ) ) ;
#996 = EDGE_LOOP ( 'NONE', ( #23679, #19613, #11944, #25991 ) ) ;
#997 = DIRECTION ( 'NONE',  ( 0.000000000000000000, 0.000000000000000000, 1.000000000000000000 ) ) ;
#998 = CARTESIAN_POINT ( 'NONE',  ( -0.3012109481301850633, 0.3598698725862389813, 0.07637795275590551769 ) ) ;
#999 = CARTESIAN_POINT ( 'NONE',  ( -0.6187452617803784749, -0.1345185900882266972, 0.2292394813352827132 ) ) ;
#1000 = DIRECTION ( 'NONE',  ( 0.000000000000000000, -1.000000000000000000, 0.000000000000000000 ) ) ;
#1001 = EDGE_CURVE ( 'NONE', #12118, #10287, #27735, .T. ) ;
#1002 = CARTESIAN_POINT ( 'NONE',  ( 0.000000000000000000, 0.000000000000000000, 2.504921259842519898 ) ) ;
#1003 = CARTESIAN_POINT ( 'NONE',  ( 0.000000000000000000, 0.4724409448818898127, 0.000000000000000000 ) ) ;
#1004 = CARTESIAN_POINT ( 'NONE',  ( 0.1490609433494345659, -0.4786070381568058862, -0.004730797288060355210 ) ) ;
#1005 = ORIENTED_EDGE ( 'NONE', *, *, #22105, .F. ) ;
#1006 = AXIS2_PLACEMENT_3D ( 'NONE', #24971, #1119, #11840 ) ;
#1007 = ORIENTED_EDGE ( 'NONE', *, *, #24560, .F. ) ;
#1008 = CARTESIAN_POINT ( 'NONE',  ( -0.3223547283257516272, 0.3832433309296771617, 0.09685039370078740717 ) ) ;
#1009 = PLANE ( 'NONE',  #9843 ) ;
#1010 = CARTESIAN_POINT ( 'NONE',  ( 0.02061007003135870153, 0.1968503937007873850, -3.624919108234744058 ) ) ;
#1011 = VERTEX_POINT ( 'NONE', #5046 ) ;
#1012 = CARTESIAN_POINT ( 'NONE',  ( 1.197070535079588716, 0.4724409448818898127, 1.197070535079588716 ) ) ;
#1013 = ORIENTED_EDGE ( 'NONE', *, *, #10554, .F. ) ;
#1014 = VECTOR ( 'NONE', #23279, 39.37007874015748143 ) ;
#1015 = DIRECTION ( 'NONE',  ( 1.000000000000000000, 0.000000000000000000, 0.000000000000000000 ) ) ;
#1016 = B_SPLINE_CURVE_WITH_KNOTS ( 'NONE', 3,
 ( #6689, #6828, #4154, #12764, #10638, #19260, #23362, #17146 ),
 .UNSPECIFIED., .F., .F.,
 ( 4, 2, 2, 4 ),
 ( 0.5000000000000000000, 0.7500000000000000000, 0.8749999999999998890, 1.000000000000000000 ),
 .UNSPECIFIED. ) ;
#1017 = DIRECTION ( 'NONE',  ( 1.000000000000000000, 0.000000000000000000, 0.000000000000000000 ) ) ;
#1018 = CARTESIAN_POINT ( 'NONE',  ( 0.7874015748031325534, 0.2490515971710990650, -0.2751036149061643621 ) ) ;
#1019 = ADVANCED_FACE ( 'NONE', ( #18015 ), #22311, .T. ) ;
#1020 = DIRECTION ( 'NONE',  ( -1.000000000000000000, 0.000000000000000000, 0.000000000000000000 ) ) ;
#1021 = PRODUCT_RELATED_PRODUCT_CATEGORY ( 'part', '', ( #27628 ) ) ;
#1022 = ORIENTED_EDGE ( 'NONE', *, *, #21337, .F. ) ;
#1023 = ORIENTED_EDGE ( 'NONE', *, *, #2966, .T. ) ;
#1024 = CARTESIAN_POINT ( 'NONE',  ( -0.04380447413658894451, -0.3324885138898239778, 1.973425196850393970 ) ) ;
#1025 = CARTESIAN_POINT ( 'NONE',  ( -0.4921259842519975503, -0.03220957031763956036, -1.550196850393700920 ) ) ;
#1026 = ADVANCED_FACE ( 'NONE', ( #5184 ), #7886, .F. ) ;
#1027 = AXIS2_PLACEMENT_3D ( 'NONE', #3554, #3412, #20244 ) ;
#1028 = DIRECTION ( 'NONE',  ( 0.000000000000000000, 0.000000000000000000, -1.000000000000000000 ) ) ;
#1029 = CARTESIAN_POINT ( 'NONE',  ( -0.4152525734086685016, 0.3642352168757148623, 0.9399606299212598381 ) ) ;
#1030 = CIRCLE ( 'NONE', #19050, 0.8162224727389330026 ) ;
#1031 = DIRECTION ( 'NONE',  ( 0.000000000000000000, 0.000000000000000000, 1.000000000000000000 ) ) ;
#1032 = ADVANCED_FACE ( 'NONE', ( #22429 ), #17495, .T. ) ;
#1033 = EDGE_CURVE ( 'NONE', #17335, #10511, #12376, .T. ) ;
#1034 = CARTESIAN_POINT ( 'NONE',  ( -0.5905511811023621549, 0.6995255587508188988, 8.566717364459539934E-17 ) ) ;
#1035 = ORIENTED_EDGE ( 'NONE', *, *, #1061, .T. ) ;
#1036 = CARTESIAN_POINT ( 'NONE',  ( 0.000000000000000000, 0.000000000000000000, 0.1992125984251968684 ) ) ;
#1037 = CARTESIAN_POINT ( 'NONE',  ( -0.2180862235769353841, 0.4423390553432505756, -1.569881889763779625 ) ) ;
#1038 = AXIS2_PLACEMENT_3D ( 'NONE', #13010, #9304, #25877 ) ;
#1039 = DIRECTION ( 'NONE',  ( 0.000000000000000000, 0.000000000000000000, 1.000000000000000000 ) ) ;
#1040 = CARTESIAN_POINT ( 'NONE',  ( 0.1707210962531913734, -0.4707890492249701131, 0.2574803149606298969 ) ) ;
#1041 = DIRECTION ( 'NONE',  ( 0.000000000000000000, -1.000000000000000000, 0.000000000000000000 ) ) ;
#1042 = CARTESIAN_POINT ( 'NONE',  ( 0.3998447049182889956, 0.4754871227240441423, 0.2574803149606298969 ) ) ;
#1043 = ORIENTED_EDGE ( 'NONE', *, *, #4237, .T. ) ;
#1044 = DIRECTION ( 'NONE',  ( 1.000000000000000000, 0.000000000000000000, 0.000000000000000000 ) ) ;
#1045 = PRODUCT_DEFINITION_SHAPE ( 'NONE', 'NONE',  #27913 ) ;
#1046 = DIRECTION ( 'NONE',  ( 0.000000000000000000, 0.000000000000000000, 1.000000000000000000 ) ) ;
#1047 = VERTEX_POINT ( 'NONE', #15795 ) ;
#1048 = AXIS2_PLACEMENT_3D ( 'NONE', #23857, #19612, #2759 ) ;
#1049 = CARTESIAN_POINT ( 'NONE',  ( -0.0003454908279975151160, 0.3771652360013086902, 0.07637630750536809898 ) ) ;
#1050 = ORIENTED_EDGE ( 'NONE', *, *, #16246, .F. ) ;
#1051 = ( BOUNDED_CURVE ( )  B_SPLINE_CURVE ( 2, ( #18464, #13977, #3211 ),
 .UNSPECIFIED., .F., .T. ) 
 B_SPLINE_CURVE_WITH_KNOTS ( ( 3, 3 ),
 ( 0.000000000000000000, 0.2336872276155829986 ),
 .UNSPECIFIED. ) 
 CURVE ( )  GEOMETRIC_REPRESENTATION_ITEM ( )  RATIONAL_B_SPLINE_CURVE ( ( 1.000000000000000000, 1.154700538379245911, 1.000000000000000000 ) ) 
 REPRESENTATION_ITEM ( '' )  ) ;
#1052 = CARTESIAN_POINT ( 'NONE',  ( -0.3929158813954686247, -0.2268989272875759633, -1.934055118110236338 ) ) ;
#1053 = CIRCLE ( 'NONE', #16846, 0.1082677165354330312 ) ;
#1054 = CARTESIAN_POINT ( 'NONE',  ( -0.09842519685039370636, -0.07874015748031495954, 0.04546065111729338803 ) ) ;
#1055 = FACE_BOUND ( 'NONE', #16566, .T. ) ;
#1056 = CARTESIAN_POINT ( 'NONE',  ( -0.04991389860279011464, 0.3112157083527658519, -3.186815069313337023 ) ) ;
#1057 = DIRECTION ( 'NONE',  ( 0.000000000000000000, 0.000000000000000000, -1.000000000000000000 ) ) ;
#1058 = CARTESIAN_POINT ( 'NONE',  ( 0.3543307086614173040, 0.09842519685039370636, 0.000000000000000000 ) ) ;
#1059 = ORIENTED_EDGE ( 'NONE', *, *, #21507, .T. ) ;
#1060 = DIRECTION ( 'NONE',  ( 1.000000000000000000, 0.000000000000000000, 0.000000000000000000 ) ) ;
#1061 = EDGE_CURVE ( 'NONE', #11368, #24827, #15560, .T. ) ;
#1062 = VECTOR ( 'NONE', #24990, 39.37007874015748143 ) ;
#1063 = CARTESIAN_POINT ( 'NONE',  ( -0.2274877609455561167, -0.4708572476080006841, 0.1392975274314397494 ) ) ;
#1064 = VERTEX_POINT ( 'NONE', #15664 ) ;
#1065 = CARTESIAN_POINT ( 'NONE',  ( -0.3702005978258584573, -0.04877294052295926691, -3.115157480314960647 ) ) ;
#1066 = CIRCLE ( 'NONE', #3291, 0.06200787401574806013 ) ;
#1067 = DIRECTION ( 'NONE',  ( -0.2225209339563148925, -0.9749279121818235083, 0.000000000000000000 ) ) ;
#1068 = EDGE_CURVE ( 'NONE', #24735, #4219, #15983, .T. ) ;
#1069 = EDGE_LOOP ( 'NONE', ( #7141, #12529 ) ) ;
#1070 = CARTESIAN_POINT ( 'NONE',  ( 0.3535065162672724748, -0.2712027394948692827, -1.934055118110236338 ) ) ;
#1071 = EDGE_CURVE ( 'NONE', #14592, #10766, #7407, .T. ) ;
#1072 = AXIS2_PLACEMENT_3D ( 'NONE', #797, #26485, #22259 ) ;
#1073 = CARTESIAN_POINT ( 'NONE',  ( 0.09842519685039366473, 0.1968503937007873850, -3.548228346456693050 ) ) ;
#1074 = DIRECTION ( 'NONE',  ( 0.000000000000000000, 0.000000000000000000, 1.000000000000000000 ) ) ;
#1075 = CARTESIAN_POINT ( 'NONE',  ( 0.3121994997598600552, -0.4069448477555897004, 1.766732283464566899 ) ) ;
#1076 = ORIENTED_EDGE ( 'NONE', *, *, #5071, .F. ) ;
#1077 = CARTESIAN_POINT ( 'NONE',  ( 0.4771018889076559244, 0.3804760601893846794, 0.2362204724409449064 ) ) ;
#1078 = EDGE_CURVE ( 'NONE', #21206, #27702, #25930, .T. ) ;
#1079 = ORIENTED_EDGE ( 'NONE', *, *, #19204, .T. ) ;
#1080 = CONICAL_SURFACE ( 'NONE', #17752, 0.6246466694403326469, 0.2617993874999998694 ) ;
#1081 = CARTESIAN_POINT ( 'NONE',  ( 0.09762295995069811272, -0.3644697409450263215, -3.100567304031765836 ) ) ;
#1082 = CIRCLE ( 'NONE', #11898, 0.1181102362204720091 ) ;
#1083 = FACE_OUTER_BOUND ( 'NONE', #21459, .T. ) ;
#1084 = CARTESIAN_POINT ( 'NONE',  ( 0.04115487667019134682, -0.3914832076178914044, -0.3299005569521964443 ) ) ;
#1085 = VERTEX_POINT ( 'NONE', #2918 ) ;
#1086 = VERTEX_POINT ( 'NONE', #20162 ) ;
#1087 = CARTESIAN_POINT ( 'NONE',  ( -0.3607509115914968589, -0.7060833311703261783, -0.6427979834437553830 ) ) ;
#1088 = DIRECTION ( 'NONE',  ( 0.000000000000000000, -1.000000000000000000, 0.000000000000000000 ) ) ;
#1089 = ORIENTED_EDGE ( 'NONE', *, *, #4333, .F. ) ;
#1090 = CARTESIAN_POINT ( 'NONE',  ( 0.4417361510193959506, -0.05819755867303935681, -1.934055118110236338 ) ) ;
#1091 = ORIENTED_EDGE ( 'NONE', *, *, #9443, .F. ) ;
#1092 = ORIENTED_EDGE ( 'NONE', *, *, #1886, .F. ) ;
#1093 = PLANE ( 'NONE',  #21809 ) ;
#1094 = CARTESIAN_POINT ( 'NONE',  ( 0.000000000000000000, 0.000000000000000000, 0.1322834645669291320 ) ) ;
#1095 = CIRCLE ( 'NONE', #20479, 0.08582677165167480748 ) ;
#1096 = EDGE_CURVE ( 'NONE', #24517, #18812, #4630, .T. ) ;
#1097 = CARTESIAN_POINT ( 'NONE',  ( -0.06881554280526554213, 0.1968503937007874127, -3.233007928613536919 ) ) ;
#1098 = ( NAMED_UNIT ( * ) PLANE_ANGLE_UNIT ( ) SI_UNIT ( $, .RADIAN. ) ) ;
#1099 = CARTESIAN_POINT ( 'NONE',  ( -0.3346456692913385988, 2.134256245050205639E-17, 1.973425196850393970 ) ) ;
#1100 = DIRECTION ( 'NONE',  ( 0.9790454724845839563, -0.2036417511401769909, 0.000000000000000000 ) ) ;
#1101 = EDGE_CURVE ( 'NONE', #17070, #17929, #9204, .T. ) ;
#1102 = AXIS2_PLACEMENT_3D ( 'NONE', #11901, #14175, #1443 ) ;
#1103 = CARTESIAN_POINT ( 'NONE',  ( -0.3066721922917531873, 0.000000000000000000, -0.05856299212598425896 ) ) ;
#1104 = CARTESIAN_POINT ( 'NONE',  ( -8.427884271297532088E-17, -0.6881889763779527325, -1.092739370078740131E-17 ) ) ;
#1105 = CARTESIAN_POINT ( 'NONE',  ( 0.2341512108694265570, -0.2669480828848097009, 1.953740157480315043 ) ) ;
#1106 = ORIENTED_EDGE ( 'NONE', *, *, #4796, .T. ) ;
#1107 = CARTESIAN_POINT ( 'NONE',  ( -2.073220866141732523E-16, 0.07874015748031495954, 1.574803149606299524 ) ) ;
#1108 = CARTESIAN_POINT ( 'NONE',  ( -0.3453142639840502404, -1.185886736896986315, -0.5421347595288529275 ) ) ;
#1109 = EDGE_CURVE ( 'NONE', #8913, #147, #3613, .T. ) ;
#1110 = DIRECTION ( 'NONE',  ( -0.8660254037844385966, -0.5000000000000002220, 0.000000000000000000 ) ) ;
#1111 = CARTESIAN_POINT ( 'NONE',  ( 0.7874015748031496509, -0.6060691875862894706, 0.08482860590294842573 ) ) ;
#1112 = CARTESIAN_POINT ( 'NONE',  ( 0.4441657790107724213, -0.2564944395515492137, 1.747047244094488194 ) ) ;
#1113 = CARTESIAN_POINT ( 'NONE',  ( 0.3855916753051445989, -0.3382184156732112590, 1.766732283464566899 ) ) ;
#1114 = AXIS2_PLACEMENT_3D ( 'NONE', #7079, #15697, #24300 ) ;
#1115 = ORIENTED_EDGE ( 'NONE', *, *, #12278, .F. ) ;
#1116 = CARTESIAN_POINT ( 'NONE',  ( 0.1589886963209722337, -0.4351482077926094871, 0.1494804571181609920 ) ) ;
#1117 = EDGE_LOOP ( 'NONE', ( #20134, #3108, #1, #19528 ) ) ;
#1118 = CARTESIAN_POINT ( 'NONE',  ( 0.6708784387195235732, -0.1533826961018693036, 0.3401599409343967761 ) ) ;
#1119 = DIRECTION ( 'NONE',  ( 0.3420201433256691570, 0.9396926207859084279, -0.000000000000000000 ) ) ;
#1120 = FACE_OUTER_BOUND ( 'NONE', #1478, .T. ) ;
#1121 = ORIENTED_EDGE ( 'NONE', *, *, #6645, .T. ) ;
#1122 = EDGE_LOOP ( 'NONE', ( #10970, #9534, #26213, #4529, #19127, #25779 ) ) ;
#1123 = CARTESIAN_POINT ( 'NONE',  ( -0.3001918266902340870, -0.3912931228432089403, -1.569881889763779625 ) ) ;
#1124 = AXIS2_PLACEMENT_3D ( 'NONE', #13348, #15489, #11366 ) ;
#1125 = ORIENTED_EDGE ( 'NONE', *, *, #21190, .F. ) ;
#1126 = EDGE_LOOP ( 'NONE', ( #5710, #17595 ) ) ;
#1127 = ITEM_DEFINED_TRANSFORMATION ( 'NONE', 'NONE', #15248,  #11588 ) ;
#1128 = DIRECTION ( 'NONE',  ( 1.000000000000000000, 0.000000000000000000, 0.000000000000000000 ) ) ;
#1129 = CARTESIAN_POINT ( 'NONE',  ( -0.5850448763834590338, 0.000000000000000000, -0.2755905511811023723 ) ) ;
#1130 = CARTESIAN_POINT ( 'NONE',  ( 0.1516263115863346334, 0.4909405214979283838, 0.05579628926458630317 ) ) ;
#1131 = CARTESIAN_POINT ( 'NONE',  ( -0.3338887748335582772, -5.862181872598426086E-06, -1.869015748010449007 ) ) ;
#1132 = EDGE_CURVE ( 'NONE', #24679, #11735, #20131, .T. ) ;
#1133 = AXIS2_PLACEMENT_3D ( 'NONE', #26214, #24367, #4873 ) ;
#1134 = EDGE_CURVE ( 'NONE', #2754, #5280, #13734, .T. ) ;
#1135 = CARTESIAN_POINT ( 'NONE',  ( 0.000000000000000000, 0.000000000000000000, -0.1377952755696461029 ) ) ;
#1136 = CARTESIAN_POINT ( 'NONE',  ( -0.1677079028045393438, -0.2904160862623708095, 1.953740157480315043 ) ) ;
#1137 = B_SPLINE_CURVE_WITH_KNOTS ( 'NONE', 3,
 ( #26836, #22317, #13559, #16110, #2949, #11581, #1140, #9447, #18338, #998 ),
 .UNSPECIFIED., .F., .F.,
 ( 4, 2, 2, 2, 4 ),
 ( 0.000000000000000000, 0.2500000000000000000, 0.5000000000000000000, 0.7500000000000000000, 1.000000000000000000 ),
 .UNSPECIFIED. ) ;
#1138 = ORIENTED_EDGE ( 'NONE', *, *, #4001, .T. ) ;
#1139 = DIRECTION ( 'NONE',  ( 0.000000000000000000, 0.000000000000000000, 1.000000000000000000 ) ) ;
#1140 = CARTESIAN_POINT ( 'NONE',  ( -0.3191377210036941414, 0.3812612458990542463, 0.1140743250907937795 ) ) ;
#1141 = TOROIDAL_SURFACE ( 'NONE', #20078, 0.6102362204724409711, 0.1299212598425196763 ) ;
#1142 = CARTESIAN_POINT ( 'NONE',  ( -0.6119659649693193204, -0.1584167327113908397, 0.2264510984896760670 ) ) ;
#1143 = CIRCLE ( 'NONE', #10607, 0.1082677165354330312 ) ;
#1144 = FACE_OUTER_BOUND ( 'NONE', #12935, .T. ) ;
#1145 = CARTESIAN_POINT ( 'NONE',  ( -0.3135473077061334268, 0.000000000000000000, 2.504921259842519898 ) ) ;
#1146 = CARTESIAN_POINT ( 'NONE',  ( 0.1512183756280983948, -0.4867863319339438277, -0.04701115990130280697 ) ) ;
#1147 = ORIENTED_EDGE ( 'NONE', *, *, #20181, .T. ) ;
#1148 = LENGTH_MEASURE_WITH_UNIT ( LENGTH_MEASURE( 0.02539999999999999897 ), #16121 ) ;
#1149 = AXIS2_PLACEMENT_3D ( 'NONE', #9958, #18559, #8409 ) ;
#1150 = ORIENTED_EDGE ( 'NONE', *, *, #8559, .T. ) ;
#1151 = DIRECTION ( 'NONE',  ( 0.000000000000000000, -1.000000000000000000, 0.000000000000000000 ) ) ;
#1152 = DIRECTION ( 'NONE',  ( -0.2588190448135640476, 0.000000000000000000, -0.9659258263664939337 ) ) ;
#1153 = CARTESIAN_POINT ( 'NONE',  ( 0.03965503742771005202, 0.1968503937007873850, -3.617030424444199088 ) ) ;
#1154 = APPLICATION_CONTEXT ( 'automotive_design' ) ;
#1155 = ORIENTED_EDGE ( 'NONE', *, *, #18449, .F. ) ;
#1156 = CARTESIAN_POINT ( 'NONE',  ( -0.07874015748031502893, 0.1968503937007874127, -3.272637795275590733 ) ) ;
#1157 = ORIENTED_EDGE ( 'NONE', *, *, #4766, .T. ) ;
#1158 = CIRCLE ( 'NONE', #19655, 0.3740157480314960647 ) ;
#1159 = CARTESIAN_POINT ( 'NONE',  ( -0.1968503937007874127, 0.000000000000000000, 0.000000000000000000 ) ) ;
#1160 = ADVANCED_FACE ( 'NONE', ( #25108, #24822 ), #23001, .T. ) ;
#1161 = CIRCLE ( 'NONE', #15602, 0.8031496062992127261 ) ;
#1162 = ADVANCED_FACE ( 'NONE', ( #9991 ), #18161, .F. ) ;
#1163 = AXIS2_PLACEMENT_3D ( 'NONE', #5767, #10124, #27373 ) ;
#1164 = FACE_OUTER_BOUND ( 'NONE', #3351, .T. ) ;
#1165 = VERTEX_POINT ( 'NONE', #5771 ) ;
#1166 = CARTESIAN_POINT ( 'NONE',  ( 0.000000000000000000, 0.000000000000000000, 0.1377952755905511584 ) ) ;
#1167 = ORIENTED_EDGE ( 'NONE', *, *, #24794, .F. ) ;
#1168 = EDGE_LOOP ( 'NONE', ( #2501, #9246, #14088, #7714 ) ) ;
#1169 = CARTESIAN_POINT ( 'NONE',  ( -0.3007905576423873240, 0.1482986320106437494, 1.973425196850393970 ) ) ;
#1170 = VECTOR ( 'NONE', #19085, 39.37007874015748143 ) ;
#1171 = CARTESIAN_POINT ( 'NONE',  ( -0.1285103288269285327, -0.3545966721392122545, 0.1992125984251968684 ) ) ;
#1172 = CARTESIAN_POINT ( 'NONE',  ( 0.5335524835332355886, 0.1429116519061127411, 0.9202755905511811330 ) ) ;
#1173 = CARTESIAN_POINT ( 'NONE',  ( -0.4771018889076559244, 0.3804760601893846794, 0.2362204724409449064 ) ) ;
#1174 = CARTESIAN_POINT ( 'NONE',  ( 0.1601448837025507554, -0.4411213145380000200, 0.07637630773773071424 ) ) ;
#1175 = ORIENTED_EDGE ( 'NONE', *, *, #10870, .F. ) ;
#1176 = CARTESIAN_POINT ( 'NONE',  ( -0.009795313329799356164, 0.08526597544922019656, -0.4724409448841456749 ) ) ;
#1177 = CARTESIAN_POINT ( 'NONE',  ( 0.03220957031753989008, 0.4921259842519685179, -1.569881889763779625 ) ) ;
#1178 = CARTESIAN_POINT ( 'NONE',  ( 0.000000000000000000, 0.03937007874015751446, 0.5511811023975373702 ) ) ;
#1179 = TOROIDAL_SURFACE ( 'NONE', #8830, 0.4232283464566928832, 0.07677165354330708902 ) ;
#1180 = FACE_OUTER_BOUND ( 'NONE', #1413, .T. ) ;
#1181 = LENGTH_MEASURE_WITH_UNIT ( LENGTH_MEASURE( 0.02539999999999999897 ), #9208 ) ;
#1182 = ADVANCED_FACE ( 'NONE', ( #9849 ), #22775, .T. ) ;
#1183 = DIRECTION ( 'NONE',  ( 0.000000000000000000, 0.000000000000000000, -1.000000000000000000 ) ) ;
#1184 = ORIENTED_EDGE ( 'NONE', *, *, #12547, .T. ) ;
#1185 = ORIENTED_EDGE ( 'NONE', *, *, #7200, .F. ) ;
#1186 = EDGE_CURVE ( 'NONE', #12297, #1011, #18232, .T. ) ;
#1187 = VECTOR ( 'NONE', #1591, 39.37007874015748143 ) ;
#1188 = CARTESIAN_POINT ( 'NONE',  ( 0.9842519685039370358, -2.559055118110236560, 0.2952755905511810774 ) ) ;
#1189 = DIRECTION ( 'NONE',  ( -0.9790454724845842893, 0.2036417511401760472, 0.000000000000000000 ) ) ;
#1190 = CARTESIAN_POINT ( 'NONE',  ( -0.08582677165167483524, 0.000000000000000000, -0.4724409448818898127 ) ) ;
#1191 = ORIENTED_EDGE ( 'NONE', *, *, #24120, .T. ) ;
#1192 = CARTESIAN_POINT ( 'NONE',  ( 0.3184597017669858476, 0.1570773243922341800, 1.953740157480315043 ) ) ;
#1193 = ORIENTED_EDGE ( 'NONE', *, *, #9457, .F. ) ;
#1194 = CARTESIAN_POINT ( 'NONE',  ( -0.4382752542995838052, -0.1173917140416377847, -1.934055118110236338 ) ) ;
#1195 = DIRECTION ( 'NONE',  ( 0.000000000000000000, 0.000000000000000000, 1.000000000000000000 ) ) ;
#1196 = CARTESIAN_POINT ( 'NONE',  ( 0.07874794988990475864, 0.3051012802738558571, -3.212194302032695070 ) ) ;
#1197 = FACE_OUTER_BOUND ( 'NONE', #10306, .T. ) ;
#1198 = DIRECTION ( 'NONE',  ( -1.000000000000000000, 0.000000000000000000, 0.000000000000000000 ) ) ;
#1199 = DIRECTION ( 'NONE',  ( -0.6427876096865393629, 0.7660444431189780135, 0.000000000000000000 ) ) ;
#1200 = ORIENTED_EDGE ( 'NONE', *, *, #18449, .T. ) ;
#1201 = CARTESIAN_POINT ( 'NONE',  ( -0.2420394123212937232, 0.2892587550802429575, 0.1992125984251968684 ) ) ;
#1202 = DIRECTION ( 'NONE',  ( 0.000000000000000000, 1.000000000000000000, 0.000000000000000000 ) ) ;
#1203 = VERTEX_POINT ( 'NONE', #5482 ) ;
#1204 = CARTESIAN_POINT ( 'NONE',  ( -0.3384212623783144913, -0.1668516812751341671, -3.100567304031760951 ) ) ;
#1205 = VECTOR ( 'NONE', #24148, 39.37007874015748143 ) ;
#1206 = EDGE_LOOP ( 'NONE', ( #20592, #15757, #18634, #4273, #12078, #24003 ) ) ;
#1207 = CARTESIAN_POINT ( 'NONE',  ( -0.2761764805255799704, 0.3599896729929456529, -1.934055118110236338 ) ) ;
#1208 = EDGE_CURVE ( 'NONE', #4395, #4877, #8780, .T. ) ;
#1209 = ORIENTED_EDGE ( 'NONE', *, *, #27427, .F. ) ;
#1210 = CARTESIAN_POINT ( 'NONE',  ( -0.4473595089310440920, -0.4824549569468952748, -0.3934827063516405654 ) ) ;
#1211 = DIRECTION ( 'NONE',  ( 1.000000000000000000, 0.000000000000000000, 0.000000000000000000 ) ) ;
#1212 = CARTESIAN_POINT ( 'NONE',  ( 0.06957181182498554939, 0.5280699926562867352, 1.747047244094488194 ) ) ;
#1213 = CARTESIAN_POINT ( 'NONE',  ( 0.000000000000000000, 0.000000000000000000, 0.2374015748031496065 ) ) ;
#1214 = EDGE_LOOP ( 'NONE', ( #23740, #11327, #1147, #4046 ) ) ;
#1215 = ADVANCED_FACE ( 'NONE', ( #11828 ), #5648, .F. ) ;
#1216 = DIRECTION ( 'NONE',  ( 0.000000000000000000, 1.224646799147352221E-16, 1.000000000000000000 ) ) ;
#1217 = CARTESIAN_POINT ( 'NONE',  ( -0.1213180142433868958, -0.3572819248074448062, -3.100567304031760951 ) ) ;
#1218 = AXIS2_PLACEMENT_3D ( 'NONE', #22516, #18393, #22374 ) ;
#1219 = EDGE_CURVE ( 'NONE', #15450, #13929, #14689, .T. ) ;
#1220 = LINE ( 'NONE', #9824, #25523 ) ;
#1221 = PRODUCT_DEFINITION_SHAPE ( 'NONE', 'NONE',  #2566 ) ;
#1222 = CARTESIAN_POINT ( 'NONE',  ( 0.000000000000000000, 0.4724409448818898127, 1.377952755905512472 ) ) ;
#1223 = EDGE_CURVE ( 'NONE', #6621, #1203, #26524, .T. ) ;
#1224 = EDGE_LOOP ( 'NONE', ( #22539, #14658 ) ) ;
#1225 = CIRCLE ( 'NONE', #8422, 0.003937007874015747977 ) ;
#1226 = CARTESIAN_POINT ( 'NONE',  ( -0.4315274442044927383, -0.5217045752503943756, -0.4246611536723189917 ) ) ;
#1227 = DIRECTION ( 'NONE',  ( 1.000000000000000000, 0.000000000000000000, 0.000000000000000000 ) ) ;
#1228 = EDGE_CURVE ( 'NONE', #3526, #26154, #15140, .T. ) ;
#1229 = B_SPLINE_CURVE_WITH_KNOTS ( 'NONE', 3,
 ( #14885, #198, #17116, #11030, #325, #8767 ),
 .UNSPECIFIED., .F., .F.,
 ( 4, 2, 4 ),
 ( 0.3000437156586439613, 0.3015484798814569989, 0.3030532441042709801 ),
 .UNSPECIFIED. ) ;
#1230 = CARTESIAN_POINT ( 'NONE',  ( 0.3535065162672720307, 0.2712027394948698378, -1.934055118110236338 ) ) ;
#1231 = VERTEX_POINT ( 'NONE', #23141 ) ;
#1232 = ORIENTED_EDGE ( 'NONE', *, *, #23960, .F. ) ;
#1233 = CARTESIAN_POINT ( 'NONE',  ( -0.7874015748031496509, 0.4828108945773819105, 0.1423708153504031348 ) ) ;
#1234 = DIRECTION ( 'NONE',  ( -1.000000000000000000, 0.000000000000000000, 0.000000000000000000 ) ) ;
#1235 = CARTESIAN_POINT ( 'NONE',  ( 0.2180698645301765992, 0.2842490391651533721, -3.115157480314960647 ) ) ;
#1236 = DIRECTION ( 'NONE',  ( 0.000000000000000000, 0.000000000000000000, 1.000000000000000000 ) ) ;
#1237 = B_SPLINE_CURVE_WITH_KNOTS ( 'NONE', 3,
 ( #6570, #10655, #1901, #23804, #17029, #25640 ),
 .UNSPECIFIED., .F., .F.,
 ( 4, 2, 4 ),
 ( 1.217380381967464009, 1.219305002860850085, 1.221229623754233939 ),
 .UNSPECIFIED. ) ;
#1238 = CARTESIAN_POINT ( 'NONE',  ( 0.2952755905511810774, 0.000000000000000000, 0.2637795275590551491 ) ) ;
#1239 = CARTESIAN_POINT ( 'NONE',  ( -0.1141732283464566844, 0.000000000000000000, 0.000000000000000000 ) ) ;
#1240 = CARTESIAN_POINT ( 'NONE',  ( 0.4535326485287339282, 0.08054850140356757671, 0.1771653543307084855 ) ) ;
#1241 = CARTESIAN_POINT ( 'NONE',  ( 0.1516263115863346334, -0.1971492568089275588, -0.4530651079966787620 ) ) ;
#1242 = EDGE_LOOP ( 'NONE', ( #16794, #2990 ) ) ;
#1243 = CARTESIAN_POINT ( 'NONE',  ( -0.7214243740396926174, -0.1654689342655534801, 0.2161412452766471592 ) ) ;
#1244 = FACE_OUTER_BOUND ( 'NONE', #1397, .T. ) ;
#1245 = CARTESIAN_POINT ( 'NONE',  ( -0.6562077975700374433, -1.365924015748031427E-17, -0.2362204724409449064 ) ) ;
#1246 = CARTESIAN_POINT ( 'NONE',  ( 0.4225965726692672009, 0.3242071728275124354, 1.747047244094488194 ) ) ;
#1247 = LINE ( 'NONE', #7602, #6111 ) ;
#1248 = CARTESIAN_POINT ( 'NONE',  ( -0.1327036767659643679, -0.4954415918530851726, 1.766732283464566899 ) ) ;
#1249 = EDGE_CURVE ( 'NONE', #21158, #7057, #2465, .T. ) ;
#1250 = EDGE_LOOP ( 'NONE', ( #8180, #21295, #4670, #1522 ) ) ;
#1251 = CARTESIAN_POINT ( 'NONE',  ( -0.3392387706403475200, 0.1151913129404399938, -3.115157480314960647 ) ) ;
#1252 = ORIENTED_EDGE ( 'NONE', *, *, #21408, .T. ) ;
#1253 = CARTESIAN_POINT ( 'NONE',  ( 0.2255758929755326547, -0.6217623271420399389, 0.1616495878830931654 ) ) ;
#1254 = DIRECTION ( 'NONE',  ( 1.000000000000000000, 0.000000000000000000, 0.000000000000000000 ) ) ;
#1255 = CARTESIAN_POINT ( 'NONE',  ( 0.000000000000000000, 0.000000000000000000, 0.01181102362204724393 ) ) ;
#1256 = ADVANCED_FACE ( 'NONE', ( #5909 ), #16077, .T. ) ;
#1257 = CARTESIAN_POINT ( 'NONE',  ( -0.4173606904761050229, 0.000000000000000000, -0.1464516454673935042 ) ) ;
#1258 = EDGE_LOOP ( 'NONE', ( #23878, #2968, #26517, #23453 ) ) ;
#1259 = ORIENTED_EDGE ( 'NONE', *, *, #11342, .T. ) ;
#1260 = CARTESIAN_POINT ( 'NONE',  ( 0.4921259842519685179, -0.03220957031753991784, -1.569881889763779625 ) ) ;
#1261 = ( GEOMETRIC_REPRESENTATION_CONTEXT ( 3 ) GLOBAL_UNCERTAINTY_ASSIGNED_CONTEXT ( ( #4018 ) ) GLOBAL_UNIT_ASSIGNED_CONTEXT ( ( #20102, #7243, #11487 ) ) REPRESENTATION_CONTEXT ( 'NONE', 'WORKASPACE' ) ) ;
#1262 = CONICAL_SURFACE ( 'NONE', #22899, 0.4526932812344527379, 0.1178097243749990780 ) ;
#1263 = ORIENTED_EDGE ( 'NONE', *, *, #3666, .T. ) ;
#1264 = ORIENTED_EDGE ( 'NONE', *, *, #20212, .F. ) ;
#1265 = ORIENTED_EDGE ( 'NONE', *, *, #26244, .T. ) ;
#1266 = CARTESIAN_POINT ( 'NONE',  ( 0.6791338582677166613, 0.000000000000000000, 0.000000000000000000 ) ) ;
#1267 = CARTESIAN_POINT ( 'NONE',  ( 0.3574975638436101444, 4.268512490100411279E-17, -3.115157480314960647 ) ) ;
#1268 = DIRECTION ( 'NONE',  ( 0.000000000000000000, -1.000000000000000000, 0.000000000000000000 ) ) ;
#1269 = CARTESIAN_POINT ( 'NONE',  ( -0.3937007874015748254, 4.821444091131312140E-17, -1.934055118110236338 ) ) ;
#1270 = FACE_OUTER_BOUND ( 'NONE', #4883, .T. ) ;
#1271 = CIRCLE ( 'NONE', #26511, 0.7165354330708662012 ) ;
#1272 = CARTESIAN_POINT ( 'NONE',  ( 0.000000000000000000, 0.000000000000000000, 0.3059055118110236560 ) ) ;
#1273 = CARTESIAN_POINT ( 'NONE',  ( 0.4167985568850881561, 0.07349283109919289847, 0.06102165354330708891 ) ) ;
#1274 = AXIS2_PLACEMENT_3D ( 'NONE', #25770, #19410, #16283 ) ;
#1275 = CARTESIAN_POINT ( 'NONE',  ( 0.1755067523729419432, 0.3028750839302634112, -0.5245950337139054787 ) ) ;
#1276 = CIRCLE ( 'NONE', #19786, 0.3346456692913385988 ) ;
#1277 = DIRECTION ( 'NONE',  ( 1.000000000000000000, 0.000000000000000000, 0.000000000000000000 ) ) ;
#1278 = PRODUCT_DEFINITION_SHAPE ( 'NONE', 'NONE',  #27896 ) ;
#1279 = DIRECTION ( 'NONE',  ( 1.000000000000000000, 0.000000000000000000, -0.000000000000000000 ) ) ;
#1280 = EDGE_CURVE ( 'NONE', #12816, #3515, #3825, .T. ) ;
#1281 = ORIENTED_EDGE ( 'NONE', *, *, #26449, .F. ) ;
#1282 = CARTESIAN_POINT ( 'NONE',  ( 0.2956505864974371400, 0.3532288989643546651, 0.1771653543307085410 ) ) ;
#1283 = VECTOR ( 'NONE', #10032, 39.37007874015748143 ) ;
#1284 = ORIENTED_EDGE ( 'NONE', *, *, #15743, .T. ) ;
#1285 = ADVANCED_FACE ( 'NONE', ( #11976, #20594 ), #16633, .T. ) ;
#1286 = ORIENTED_EDGE ( 'NONE', *, *, #4049, .F. ) ;
#1287 = CARTESIAN_POINT ( 'NONE',  ( -0.1771653543307086520, 0.000000000000000000, 0.000000000000000000 ) ) ;
#1288 = CARTESIAN_POINT ( 'NONE',  ( 0.1522836969735571200, 0.4941010236220468865, 0.01864847287710773294 ) ) ;
#1289 = ORIENTED_EDGE ( 'NONE', *, *, #12310, .T. ) ;
#1290 = FACE_OUTER_BOUND ( 'NONE', #17007, .T. ) ;
#1291 = ORIENTED_EDGE ( 'NONE', *, *, #14066, .F. ) ;
#1292 = CIRCLE ( 'NONE', #4886, 0.5118110236220472231 ) ;
#1293 = CARTESIAN_POINT ( 'NONE',  ( -0.2161007281675216829, -0.5956855348323873978, 0.2481708550952000381 ) ) ;
#1294 = AXIS2_PLACEMENT_3D ( 'NONE', #5908, #12769, #14538 ) ;
#1295 = MECHANICAL_DESIGN_GEOMETRIC_PRESENTATION_REPRESENTATION (  '', ( #17528 ), #411 ) ;
#1296 = CARTESIAN_POINT ( 'NONE',  ( 0.3334645669291338987, -9.254566434606299706E-06, -2.341456692880161228 ) ) ;
#1297 = DIRECTION ( 'NONE',  ( 0.000000000000000000, 0.000000000000000000, 1.000000000000000000 ) ) ;
#1298 = DIRECTION ( 'NONE',  ( 0.000000000000000000, 0.000000000000000000, -1.000000000000000000 ) ) ;
#1299 = CARTESIAN_POINT ( 'NONE',  ( 0.3543307086367249448, 0.000000000000000000, -2.322834645648385710 ) ) ;
#1300 = ORIENTED_EDGE ( 'NONE', *, *, #15873, .F. ) ;
#1301 = AXIS2_PLACEMENT_3D ( 'NONE', #19572, #253, #4583 ) ;
#1302 = CARTESIAN_POINT ( 'NONE',  ( 0.000000000000000000, 0.000000000000000000, 0.1771653543307086520 ) ) ;
#1303 = CARTESIAN_POINT ( 'NONE',  ( 0.4600326175570071952, 0.2268096725200290653, -1.550196850393700920 ) ) ;
#1304 = CARTESIAN_POINT ( 'NONE',  ( 0.5368353335967095408, 0.1442704874421229244, 0.9202755905511813550 ) ) ;
#1305 = CARTESIAN_POINT ( 'NONE',  ( -0.1429116519061075785, -0.5335524835332366989, 0.9202755905511811330 ) ) ;
#1306 = CARTESIAN_POINT ( 'NONE',  ( 0.2421724791772047192, 0.2891474103999575052, 0.1992142436757342316 ) ) ;
#1307 = CARTESIAN_POINT ( 'NONE',  ( -8.427884271297532088E-17, -0.6881889763779527325, 0.06614173228346456601 ) ) ;
#1308 = ORIENTED_EDGE ( 'NONE', *, *, #23601, .T. ) ;
#1309 = DIRECTION ( 'NONE',  ( -1.000000000000000000, 0.000000000000000000, 0.000000000000000000 ) ) ;
#1310 = AXIS2_PLACEMENT_3D ( 'NONE', #22025, #2927, #13675 ) ;
#1311 = CARTESIAN_POINT ( 'NONE',  ( -0.4921259842519685179, 0.000000000000000000, -1.569881889763779625 ) ) ;
#1312 = SURFACE_SIDE_STYLE ('',( #11903 ) ) ;
#1313 = ORIENTED_EDGE ( 'NONE', *, *, #2014, .T. ) ;
#1314 = AXIS2_PLACEMENT_3D ( 'NONE', #18114, #26761, #16038 ) ;
#1315 = AXIS2_PLACEMENT_3D ( 'NONE', #21292, #9201, #22211 ) ;
#1316 = CARTESIAN_POINT ( 'NONE',  ( 0.000000000000000000, 0.000000000000000000, -0.05511811023622047168 ) ) ;
#1317 = CARTESIAN_POINT ( 'NONE',  ( 0.3511566718594107961, 0.4004902621173285215, 1.747047244094488194 ) ) ;
#1318 = ADVANCED_FACE ( 'NONE', ( #14391 ), #2030, .T. ) ;
#1319 = ORIENTED_EDGE ( 'NONE', *, *, #129, .F. ) ;
#1320 = EDGE_CURVE ( 'NONE', #51, #1745, #8572, .T. ) ;
#1322 = CARTESIAN_POINT ( 'NONE',  ( -0.3451357231661831282, 0.000000000000000000, -0.04133858267716535029 ) ) ;
#1321 = AXIS2_PLACEMENT_3D ( 'NONE', #1328, #3417, #16302 ) ;
#1323 = DIRECTION ( 'NONE',  ( 0.000000000000000000, -1.000000000000000000, 0.000000000000000000 ) ) ;
#1324 = CARTESIAN_POINT ( 'NONE',  ( -0.3002886982018051487, -0.1727973894384558229, 0.1377952755905512416 ) ) ;
#1325 = VERTEX_POINT ( 'NONE', #15223 ) ;
#1326 = CARTESIAN_POINT ( 'NONE',  ( -0.3184623230426369966, 0.1570784101599410065, 1.953740157480315487 ) ) ;
#1327 = ORIENTED_EDGE ( 'NONE', *, *, #24883, .T. ) ;
#1328 = CARTESIAN_POINT ( 'NONE',  ( 0.000000000000000000, 0.000000000000000000, 0.1322834645669291320 ) ) ;
#1329 = DIRECTION ( 'NONE',  ( 1.000000000000000000, 0.000000000000000000, 0.000000000000000000 ) ) ;
#1330 = CARTESIAN_POINT ( 'NONE',  ( 0.1501355178992943573, -0.2698857342899688705, -0.4015219628616845671 ) ) ;
#1331 = LINE ( 'NONE', #14195, #11270 ) ;
#1332 = CARTESIAN_POINT ( 'NONE',  ( 0.7874015748031496509, -0.3839064563524846596, -0.3321176343386791907 ) ) ;
#1333 = CARTESIAN_POINT ( 'NONE',  ( -0.2350342994822195442, 0.2808987121525407527, 0.1910323753003855540 ) ) ;
#1334 = CARTESIAN_POINT ( 'NONE',  ( -0.4684132450478830645, -0.1062614382955276715, 0.2362204724409449619 ) ) ;
#1335 = CARTESIAN_POINT ( 'NONE',  ( -0.4446020952038907681, 0.000000000000000000, -1.934055118110236338 ) ) ;
#1336 = ( CONVERSION_BASED_UNIT ( 'INCH', #25059 ) LENGTH_UNIT ( ) NAMED_UNIT ( #10443 ) ) ;
#1337 = VECTOR ( 'NONE', #1696, 39.37007874015748854 ) ;
#1338 = CARTESIAN_POINT ( 'NONE',  ( 0.1275996891957757451, -0.4763861460130329184, -1.569881889763779625 ) ) ;
#1339 = ORIENTED_EDGE ( 'NONE', *, *, #16589, .T. ) ;
#1340 = EDGE_CURVE ( 'NONE', #2005, #10433, #10148, .T. ) ;
#1341 = CARTESIAN_POINT ( 'NONE',  ( 0.4303822302053771365, 0.1152775731717053109, -1.934055118110236338 ) ) ;
#1342 = VERTEX_POINT ( 'NONE', #2206 ) ;
#1343 = EDGE_CURVE ( 'NONE', #22371, #24517, #19627, .T. ) ;
#1344 = CARTESIAN_POINT ( 'NONE',  ( -0.4473595089310440920, -0.5755188248839795406, -0.2663378075042964754 ) ) ;
#1345 = DIRECTION ( 'NONE',  ( 0.000000000000000000, 0.000000000000000000, 1.000000000000000000 ) ) ;
#1346 = ORIENTED_EDGE ( 'NONE', *, *, #7162, .F. ) ;
#1347 = DIRECTION ( 'NONE',  ( 1.000000000000000000, 0.000000000000000000, 0.000000000000000000 ) ) ;
#1348 = VERTEX_POINT ( 'NONE', #21008 ) ;
#1349 = CARTESIAN_POINT ( 'NONE',  ( 0.009795313329541911057, 0.08526597544697904485, -0.4724409448818898127 ) ) ;
#1350 = FACE_OUTER_BOUND ( 'NONE', #24867, .T. ) ;
#1351 = CARTESIAN_POINT ( 'NONE',  ( 0.04115487667019118723, -0.4669989807942504512, -0.1904908102188472563 ) ) ;
#1352 = ORIENTED_EDGE ( 'NONE', *, *, #11882, .T. ) ;
#1353 = CIRCLE ( 'NONE', #24413, 0.1181102362204718703 ) ;
#1354 = CARTESIAN_POINT ( 'NONE',  ( -0.3611843684950729050, -0.7048611138537562715, -0.6407005967225004595 ) ) ;
#1355 = DIRECTION ( 'NONE',  ( -1.000000000000000000, 0.000000000000000000, 0.000000000000000000 ) ) ;
#1356 = CARTESIAN_POINT ( 'NONE',  ( 0.1432577568504609655, -0.4218945342797526532, -1.934055118110236338 ) ) ;
#1357 = ORIENTED_EDGE ( 'NONE', *, *, #3422, .F. ) ;
#1358 = ORIENTED_EDGE ( 'NONE', *, *, #13176, .T. ) ;
#1359 = CARTESIAN_POINT ( 'NONE',  ( -0.4585215200179055817, 2.807634559150536355E-17, -1.928289503579156516 ) ) ;
#1360 = CARTESIAN_POINT ( 'NONE',  ( 0.1918813796216842782, -0.5271897577243779276, 0.1771653543307086520 ) ) ;
#1361 = B_SPLINE_CURVE_WITH_KNOTS ( 'NONE', 3,
 ( #7535, #1049, #3140, #9640 ),
 .UNSPECIFIED., .F., .F.,
 ( 4, 4 ),
 ( 0.2291966065698869959, 0.2305109203526903294 ),
 .UNSPECIFIED. ) ;
#1362 = CARTESIAN_POINT ( 'NONE',  ( 0.3574975638436101444, 0.02339816079119100625, -3.115157480314960647 ) ) ;
#1363 = CARTESIAN_POINT ( 'NONE',  ( 0.1279527559055118058, 0.000000000000000000, 0.000000000000000000 ) ) ;
#1364 = CARTESIAN_POINT ( 'NONE',  ( 0.08759279594700324079, 0.3259357382551449911, 1.973425196850393526 ) ) ;
#1365 = CARTESIAN_POINT ( 'NONE',  ( -0.3040421205569480145, 0.7911861580938169825, -0.8381822164908544481 ) ) ;
#1366 = EDGE_CURVE ( 'NONE', #18057, #27874, #11501, .T. ) ;
#1367 = DIRECTION ( 'NONE',  ( 1.000000000000000000, 0.000000000000000000, 0.000000000000000000 ) ) ;
#1368 = VECTOR ( 'NONE', #4932, 39.37007874015748143 ) ;
#1369 = CARTESIAN_POINT ( 'NONE',  ( 0.4535326485287340947, 0.08054850140356764610, 0.1639447408599974121 ) ) ;
#1370 = DIRECTION ( 'NONE',  ( -0.000000000000000000, -0.000000000000000000, -1.000000000000000000 ) ) ;
#1371 = EDGE_CURVE ( 'NONE', #12126, #25040, #6106, .T. ) ;
#1372 = ORIENTED_EDGE ( 'NONE', *, *, #10616, .F. ) ;
#1373 = CARTESIAN_POINT ( 'NONE',  ( -0.3771675965698903510, 0.4301570366553708613, 0.9399606299212600602 ) ) ;
#1374 = AXIS2_PLACEMENT_3D ( 'NONE', #3401, #5409, #20799 ) ;
#1375 = DIRECTION ( 'NONE',  ( 5.737213000000000442E-16, -1.000000000000000000, 0.000000000000000000 ) ) ;
#1376 = DIRECTION ( 'NONE',  ( 1.000000000000000000, 0.000000000000000000, 0.000000000000000000 ) ) ;
#1377 = EDGE_CURVE ( 'NONE', #25529, #10943, #6997, .T. ) ;
#1378 = DIRECTION ( 'NONE',  ( 1.000000000000000000, 0.000000000000000000, 0.000000000000000000 ) ) ;
#1379 = CARTESIAN_POINT ( 'NONE',  ( 0.5280699926562892887, 0.06957181182498746452, 1.747047244094488194 ) ) ;
#1380 = CARTESIAN_POINT ( 'NONE',  ( -0.3121994997598258603, -0.4069448477556126265, 1.766732283464566899 ) ) ;
#1381 = EDGE_LOOP ( 'NONE', ( #20318, #13723, #8612, #11698 ) ) ;
#1382 = DIRECTION ( 'NONE',  ( -1.000000000000000000, 0.000000000000000000, 0.000000000000000000 ) ) ;
#1383 = ORIENTED_EDGE ( 'NONE', *, *, #9079, .F. ) ;
#1384 = CARTESIAN_POINT ( 'NONE',  ( 2.664928230027803213, 0.9448818897637796255, -1.639108661417322569E-17 ) ) ;
#1385 = CARTESIAN_POINT ( 'NONE',  ( 0.2992781133268291316, -0.6197069291944922176, 0.1322834645669291320 ) ) ;
#1386 = DIRECTION ( 'NONE',  ( 0.000000000000000000, -1.000000000000000000, 0.000000000000000000 ) ) ;
#1387 = ORIENTED_EDGE ( 'NONE', *, *, #868, .F. ) ;
#1388 = VERTEX_POINT ( 'NONE', #17057 ) ;
#1389 = AXIS2_PLACEMENT_3D ( 'NONE', #415, #8594, #17214 ) ;
#1390 = CARTESIAN_POINT ( 'NONE',  ( -0.4921259842519685179, 0.000000000000000000, -1.550196850393700920 ) ) ;
#1391 = EDGE_LOOP ( 'NONE', ( #10847, #9059, #13103, #2091, #25323 ) ) ;
#1392 = CARTESIAN_POINT ( 'NONE',  ( -0.3715251363271980245, 0.06498290224717540031, 0.1992125984251968684 ) ) ;
#1393 = CARTESIAN_POINT ( 'NONE',  ( 0.2126900928101059240, -0.5837180524351401889, 0.09684793308443542803 ) ) ;
#1394 = CARTESIAN_POINT ( 'NONE',  ( 0.4620608682196346573, 0.08206165078060492779, 0.1992125984251968684 ) ) ;
#1395 = CARTESIAN_POINT ( 'NONE',  ( 0.1718374205099799101, -0.4703827404237102550, 0.2574803149606298969 ) ) ;
#1396 = ADVANCED_FACE ( 'NONE', ( #19306 ), #27299, .F. ) ;
#1397 = EDGE_LOOP ( 'NONE', ( #19459, #25159, #1953, #13540 ) ) ;
#1398 = CARTESIAN_POINT ( 'NONE',  ( -0.5811915241081616612, -0.4724399524670138684, 0.9954595399565421276 ) ) ;
#1399 = EDGE_CURVE ( 'NONE', #214, #26850, #1656, .T. ) ;
#1400 = UNCERTAINTY_MEASURE_WITH_UNIT (LENGTH_MEASURE( 1.000000000000000082E-05 ), #650, 'distance_accuracy_value', 'NONE') ;
#1401 = CARTESIAN_POINT ( 'NONE',  ( 0.2131049448084480213, -0.5835666837866708700, 0.2574803149606298969 ) ) ;
#1402 = PLANE ( 'NONE',  #15530 ) ;
#1403 = AXIS2_PLACEMENT_3D ( 'NONE', #19008, #6721, #21281 ) ;
#1404 = CARTESIAN_POINT ( 'NONE',  ( -0.5969400767949351039, -0.2109524265843517599, 0.2188413833799605912 ) ) ;
#1405 = DIRECTION ( 'NONE',  ( 0.000000000000000000, 0.000000000000000000, -1.000000000000000000 ) ) ;
#1406 = FACE_OUTER_BOUND ( 'NONE', #22178, .T. ) ;
#1407 = ADVANCED_FACE ( 'NONE', ( #8707 ), #25945, .T. ) ;
#1408 = B_SPLINE_CURVE_WITH_KNOTS ( 'NONE', 3,
 ( #24286, #18184, #26974, #22591, #568, #5506 ),
 .UNSPECIFIED., .F., .F.,
 ( 4, 2, 4 ),
 ( 0.5000000000000000000, 0.7500000000000000000, 1.000000000000000000 ),
 .UNSPECIFIED. ) ;
#1409 = EDGE_CURVE ( 'NONE', #18722, #9569, #7421, .T. ) ;
#1410 = EDGE_LOOP ( 'NONE', ( #2496, #1567, #26591, #14884 ) ) ;
#1411 = VECTOR ( 'NONE', #2531, 39.37007874015748854 ) ;
#1412 = DIRECTION ( 'NONE',  ( 1.000000000000000000, 0.000000000000000000, 0.000000000000000000 ) ) ;
#1413 = EDGE_LOOP ( 'NONE', ( #8075, #11194 ) ) ;
#1414 = DIRECTION ( 'NONE',  ( 1.000000000000000000, 0.000000000000000000, 0.000000000000000000 ) ) ;
#1415 = EDGE_CURVE ( 'NONE', #3132, #19812, #19791, .T. ) ;
#1416 = EDGE_LOOP ( 'NONE', ( #17196, #23650, #10052, #15549 ) ) ;
#1417 = FACE_OUTER_BOUND ( 'NONE', #16441, .T. ) ;
#1418 = DIRECTION ( 'NONE',  ( 0.000000000000000000, 1.000000000000000000, 0.000000000000000000 ) ) ;
#1419 = ORIENTED_EDGE ( 'NONE', *, *, #20548, .F. ) ;
#1420 = CARTESIAN_POINT ( 'NONE',  ( 0.000000000000000000, 0.000000000000000000, 0.1377952755905511861 ) ) ;
#1421 = VERTEX_POINT ( 'NONE', #8166 ) ;
#1422 = CARTESIAN_POINT ( 'NONE',  ( 0.000000000000000000, 0.000000000000000000, 0.1771653543307086520 ) ) ;
#1423 = VECTOR ( 'NONE', #6934, 39.37007874015748143 ) ;
#1424 = CARTESIAN_POINT ( 'NONE',  ( -0.0005963271530280589861, 0.4972008316414383566, 0.1615162260929405846 ) ) ;
#1425 = DIRECTION ( 'NONE',  ( 1.000000000000000000, 0.000000000000000000, 0.000000000000000000 ) ) ;
#1426 = TOROIDAL_SURFACE ( 'NONE', #22181, 0.8031496062992127261, 0.02362204724409448786 ) ;
#1427 = EDGE_CURVE ( 'NONE', #13858, #1638, #10407, .T. ) ;
#1428 = PRESENTATION_LAYER_ASSIGNMENT (  '', '', ( #27617 ) ) ;
#1429 = CARTESIAN_POINT ( 'NONE',  ( -0.0001974756197918548992, 0.5007874015748031704, 0.09684793308443542803 ) ) ;
#1430 = DIRECTION ( 'NONE',  ( 0.000000000000000000, -1.000000000000000000, 0.000000000000000000 ) ) ;
#1431 = EDGE_CURVE ( 'NONE', #19638, #3330, #1584, .T. ) ;
#1432 = ORIENTED_EDGE ( 'NONE', *, *, #27506, .F. ) ;
#1433 = CARTESIAN_POINT ( 'NONE',  ( -0.02190250779245987017, -0.3346456692913387099, 1.973425196850393970 ) ) ;
#1434 = CARTESIAN_POINT ( 'NONE',  ( -0.06699507805605005306, -0.5085118447796763697, -1.550196850393700920 ) ) ;
#1435 = EDGE_CURVE ( 'NONE', #22878, #15456, #5641, .T. ) ;
#1436 = DIRECTION ( 'NONE',  ( 0.000000000000000000, 0.000000000000000000, -1.000000000000000000 ) ) ;
#1437 = CARTESIAN_POINT ( 'NONE',  ( -0.4887136534571460689, -0.1122103150228022234, 0.3080453759528285484 ) ) ;
#1438 = CARTESIAN_POINT ( 'NONE',  ( -0.4783323773986942751, -0.2762247810518927427, 0.9399606299212598381 ) ) ;
#1439 = FACE_OUTER_BOUND ( 'NONE', #16521, .T. ) ;
#1440 = DIRECTION ( 'NONE',  ( 0.000000000000000000, 0.000000000000000000, -1.000000000000000000 ) ) ;
#1441 = ORIENTED_EDGE ( 'NONE', *, *, #12607, .F. ) ;
#1442 = B_SPLINE_SURFACE_WITH_KNOTS ( 'NONE', 2, 3, ( 
 ( #11031, #8366, #4400, #1858 ),
 ( #8629, #19657, #16981, #21497 ),
 ( #2136, #25871, #2266, #15151 ) ),
 .UNSPECIFIED., .F., .F., .F.,
 ( 3, 3 ),
 ( 4, 4 ),
 ( 0.000000000000000000, 1.000000000000000000 ),
 ( -0.006999999999999992339, 0.000000000000000000 ),
 .UNSPECIFIED. ) ;
#1443 = DIRECTION ( 'NONE',  ( 0.000000000000000000, 1.000000000000000000, 0.000000000000000000 ) ) ;
#1444 = EDGE_CURVE ( 'NONE', #22435, #24921, #647, .T. ) ;
#1445 = CARTESIAN_POINT ( 'NONE',  ( 0.3667122560601320802, -0.09855118063547688156, -3.100567304031763172 ) ) ;
#1446 = CIRCLE ( 'NONE', #16780, 0.1673228346456692994 ) ;
#1447 = CARTESIAN_POINT ( 'NONE',  ( 0.09586345222253732368, 0.2165354330708661457, -3.246875207736362956 ) ) ;
#1448 = EDGE_LOOP ( 'NONE', ( #11858, #8037, #16293, #11555 ) ) ;
#1449 = ORIENTED_EDGE ( 'NONE', *, *, #11538, .T. ) ;
#1450 = CARTESIAN_POINT ( 'NONE',  ( 0.9842519685039370358, 2.519685039370078705, 0.2952755905511810774 ) ) ;
#1451 = DIRECTION ( 'NONE',  ( -1.000000000000000000, 0.000000000000000000, 0.000000000000000000 ) ) ;
#1452 = CARTESIAN_POINT ( 'NONE',  ( 0.2078289949484099508, -0.4330237525398077936, 0.2362204724409449619 ) ) ;
#1453 = FACE_OUTER_BOUND ( 'NONE', #16309, .T. ) ;
#1454 = VERTEX_POINT ( 'NONE', #8971 ) ;
#1455 = DIRECTION ( 'NONE',  ( 1.000000000000000000, 0.000000000000000000, 0.000000000000000000 ) ) ;
#1456 = ORIENTED_EDGE ( 'NONE', *, *, #17785, .T. ) ;
#1457 = CARTESIAN_POINT ( 'NONE',  ( 0.2350342994834856425, 0.2808987121540589826, 0.08455817587923418477 ) ) ;
#1458 = CARTESIAN_POINT ( 'NONE',  ( -0.3031496062992123375, 0.000000000000000000, -0.03543307086614204404 ) ) ;
#1459 = DIRECTION ( 'NONE',  ( -1.000000000000000000, 0.000000000000000000, 0.000000000000000000 ) ) ;
#1460 = CARTESIAN_POINT ( 'NONE',  ( -0.2952755905264887182, 3.616083068046089993E-17, -3.110236220451535694 ) ) ;
#1461 = ORIENTED_EDGE ( 'NONE', *, *, #22420, .T. ) ;
#1462 = CARTESIAN_POINT ( 'NONE',  ( 0.7874015748031496509, -0.5320149438416890142, -0.05415347417759425186 ) ) ;
#1463 = ORIENTED_EDGE ( 'NONE', *, *, #27662, .F. ) ;
#1464 = CIRCLE ( 'NONE', #9132, 0.07874015748031489015 ) ;
#1465 = DIRECTION ( 'NONE',  ( 0.000000000000000000, 0.000000000000000000, 1.000000000000000000 ) ) ;
#1466 = ADVANCED_FACE ( 'NONE', ( #790 ), #23242, .F. ) ;
#1467 = AXIS2_PLACEMENT_3D ( 'NONE', #24695, #4934, #13548 ) ;
#1468 = B_SPLINE_CURVE_WITH_KNOTS ( 'NONE', 3,
 ( #6685, #13435, #24188, #6962, #11059, #6547 ),
 .UNSPECIFIED., .F., .F.,
 ( 4, 2, 4 ),
 ( 0.3108507187342960387, 0.3125269569790670166, 0.3142031952238389936 ),
 .UNSPECIFIED. ) ;
#1469 = DIRECTION ( 'NONE',  ( 0.000000000000000000, 0.000000000000000000, 1.000000000000000000 ) ) ;
#1470 = CARTESIAN_POINT ( 'NONE',  ( 0.4848217985909654137, 6.021729909607683004E-17, -0.04133858267716535029 ) ) ;
#1471 = EDGE_CURVE ( 'NONE', #15671, #13676, #13355, .T. ) ;
#1472 = VERTEX_POINT ( 'NONE', #21979 ) ;
#1473 = CARTESIAN_POINT ( 'NONE',  ( -0.1152775731717027019, -0.4303822302053992854, -1.934055118110236338 ) ) ;
#1474 = EDGE_CURVE ( 'NONE', #21273, #6542, #24194, .T. ) ;
#1475 = EDGE_LOOP ( 'NONE', ( #26767, #10716, #19172, #19322 ) ) ;
#1476 = ORIENTED_EDGE ( 'NONE', *, *, #20100, .F. ) ;
#1477 = ORIENTED_EDGE ( 'NONE', *, *, #1134, .F. ) ;
#1478 = EDGE_LOOP ( 'NONE', ( #8404, #19161 ) ) ;
#1479 = CARTESIAN_POINT ( 'NONE',  ( 0.5781866216494347954, 0.4620966632776112304, 0.2562996996002243066 ) ) ;
#1480 = CARTESIAN_POINT ( 'NONE',  ( 0.3715251363271980245, 0.06498290224717499786, 0.1992125984251968684 ) ) ;
#1481 = CARTESIAN_POINT ( 'NONE',  ( 0.4954415918530775120, -0.1327036767659478256, 1.747047244094488194 ) ) ;
#1482 = EDGE_LOOP ( 'NONE', ( #17416, #8893 ) ) ;
#1483 = DIRECTION ( 'NONE',  ( 0.000000000000000000, 1.000000000000000000, 0.000000000000000000 ) ) ;
#1484 = CIRCLE ( 'NONE', #8268, 0.6299212598425196763 ) ;
#1485 = ORIENTED_EDGE ( 'NONE', *, *, #4157, .T. ) ;
#1486 = AXIS2_PLACEMENT_3D ( 'NONE', #9366, #24771, #24355 ) ;
#1487 = CARTESIAN_POINT ( 'NONE',  ( -0.1668516812751398570, -0.3384212623783108276, -3.100567304031765392 ) ) ;
#1488 = DIRECTION ( 'NONE',  ( 0.000000000000000000, 1.000000000000000000, 0.000000000000000000 ) ) ;
#1489 = DIRECTION ( 'NONE',  ( -0.000000000000000000, -0.000000000000000000, 1.000000000000000000 ) ) ;
#1490 = CARTESIAN_POINT ( 'NONE',  ( 0.09187177619659094019, 0.3429980251342388264, 1.953740157480315043 ) ) ;
#1491 = ORIENTED_EDGE ( 'NONE', *, *, #6631, .F. ) ;
#1492 = AXIS2_PLACEMENT_3D ( 'NONE', #22889, #26835, #7774 ) ;
#1493 = CARTESIAN_POINT ( 'NONE',  ( -0.6107239227225801370, -0.1031077391523354814, -0.2427576718125873390 ) ) ;
#1495 = CARTESIAN_POINT ( 'NONE',  ( 0.07472527936311225416, 0.5671862884095085766, 0.9399606299212598381 ) ) ;
#1494 = CARTESIAN_POINT ( 'NONE',  ( -0.03532354024591893848, -0.07677165354330710290, 0.000000000000000000 ) ) ;
#1496 = FACE_OUTER_BOUND ( 'NONE', #23490, .T. ) ;
#1497 = ORIENTED_EDGE ( 'NONE', *, *, #21755, .T. ) ;
#1498 = VERTEX_POINT ( 'NONE', #23836 ) ;
#1499 = ORIENTED_EDGE ( 'NONE', *, *, #6385, .T. ) ;
#1500 = DIRECTION ( 'NONE',  ( 0.000000000000000000, 0.000000000000000000, 1.000000000000000000 ) ) ;
#1501 = CARTESIAN_POINT ( 'NONE',  ( -0.3338887748335570560, -0.8039705855317598182, -0.9107153245080098491 ) ) ;
#1502 = EDGE_CURVE ( 'NONE', #20698, #22435, #15499, .T. ) ;
#1503 = CARTESIAN_POINT ( 'NONE',  ( -0.3551931031211721379, -0.04679574315772278004, -3.115157480314960647 ) ) ;
#1504 = CARTESIAN_POINT ( 'NONE',  ( -0.09842519685039370636, -0.07874015748031495954, 0.04546065111729338803 ) ) ;
#1505 = DIRECTION ( 'NONE',  ( -1.000000000000000000, 0.000000000000000000, 0.000000000000000000 ) ) ;
#1506 = CARTESIAN_POINT ( 'NONE',  ( -0.3334645669291338987, 1.129605998290730273, -0.9896751316273187937 ) ) ;
#1507 = FACE_OUTER_BOUND ( 'NONE', #3850, .T. ) ;
#1508 = TOROIDAL_SURFACE ( 'NONE', #17296, 0.6102362204724409711, 0.1299212598425196763 ) ;
#1509 = DIRECTION ( 'NONE',  ( -1.000000000000000000, 0.000000000000000000, -0.000000000000000000 ) ) ;
#1510 = FACE_OUTER_BOUND ( 'NONE', #14210, .T. ) ;
#1511 = ORIENTED_EDGE ( 'NONE', *, *, #15544, .T. ) ;
#1512 = CARTESIAN_POINT ( 'NONE',  ( -0.5708661417322834497, 0.000000000000000000, 0.9399606299212598381 ) ) ;
#1513 = CIRCLE ( 'NONE', #14167, 0.1751968503937007815 ) ;
#1514 = CARTESIAN_POINT ( 'NONE',  ( -0.8725268807032540153, 0.000000000000000000, 0.2362204724409449619 ) ) ;
#1515 = CARTESIAN_POINT ( 'NONE',  ( 0.000000000000000000, 0.000000000000000000, 0.3401574803149606252 ) ) ;
#1516 = AXIS2_PLACEMENT_3D ( 'NONE', #8600, #17220, #167 ) ;
#1517 = DIRECTION ( 'NONE',  ( 0.000000000000000000, 0.000000000000000000, -1.000000000000000000 ) ) ;
#1518 = DIRECTION ( 'NONE',  ( 0.000000000000000000, 0.000000000000000000, 1.000000000000000000 ) ) ;
#1519 = DIRECTION ( 'NONE',  ( 0.000000000000000000, 0.000000000000000000, 1.000000000000000000 ) ) ;
#1520 = CARTESIAN_POINT ( 'NONE',  ( -0.5118110236220472231, 0.03349795313264340019, 1.766732283464566899 ) ) ;
#1521 = ORIENTED_EDGE ( 'NONE', *, *, #22805, .F. ) ;
#1522 = ORIENTED_EDGE ( 'NONE', *, *, #5885, .F. ) ;
#1523 = DIRECTION ( 'NONE',  ( 0.000000000000000000, 0.000000000000000000, 1.000000000000000000 ) ) ;
#1524 = ORIENTED_EDGE ( 'NONE', *, *, #26785, .T. ) ;
#1525 = CARTESIAN_POINT ( 'NONE',  ( -0.4078284417470132150, 0.4849914877844211936, 0.1061598535650708358 ) ) ;
#1526 = EDGE_CURVE ( 'NONE', #23608, #18057, #15118, .T. ) ;
#1527 = CARTESIAN_POINT ( 'NONE',  ( 0.000000000000000000, 0.000000000000000000, 0.4062992125984251635 ) ) ;
#1528 = AXIS2_PLACEMENT_3D ( 'NONE', #24169, #20201, #454 ) ;
#1529 = CARTESIAN_POINT ( 'NONE',  ( 0.1078280746903962500, -0.3175540113612315696, 1.973425196850393970 ) ) ;
#1530 = ORIENTED_EDGE ( 'NONE', *, *, #9947, .T. ) ;
#1531 = ORIENTED_EDGE ( 'NONE', *, *, #24469, .T. ) ;
#1532 = CARTESIAN_POINT ( 'NONE',  ( 0.1585706980422384171, -0.4669911931914537129, -1.550196850393700920 ) ) ;
#1533 = PRODUCT_DEFINITION ( 'UNKNOWN', '', #2104, #3431 ) ;
#1534 = EDGE_LOOP ( 'NONE', ( #26895, #14116, #21082, #6619 ) ) ;
#1535 = EDGE_CURVE ( 'NONE', #4856, #13865, #15573, .T. ) ;
#1536 = AXIS2_PLACEMENT_3D ( 'NONE', #16554, #14463, #7522 ) ;
#1537 = CONTEXT_DEPENDENT_SHAPE_REPRESENTATION ( #8007, #9350 ) ;
#1538 = EDGE_CURVE ( 'NONE', #8989, #14684, #13758, .T. ) ;
#1539 = EDGE_CURVE ( 'NONE', #2213, #9968, #20982, .T. ) ;
#1540 = CARTESIAN_POINT ( 'NONE',  ( 0.0004974201395668343718, 0.3464563358313495489, 0.1276989850566408180 ) ) ;
#1541 = CIRCLE ( 'NONE', #24983, 0.6614173228346456046 ) ;
#1542 = SPHERICAL_SURFACE ( 'NONE', #17946, 0.1299232283464566984 ) ;
#1543 = DIRECTION ( 'NONE',  ( 0.000000000000000000, 0.000000000000000000, -1.000000000000000000 ) ) ;
#1544 = ORIENTED_EDGE ( 'NONE', *, *, #11001, .F. ) ;
#1545 = CARTESIAN_POINT ( 'NONE',  ( 0.000000000000000000, 0.000000000000000000, 0.09685039370078740717 ) ) ;
#1546 = CIRCLE ( 'NONE', #3787, 2.066929133858267598 ) ;
#1547 = DIRECTION ( 'NONE',  ( 0.000000000000000000, 0.000000000000000000, 1.000000000000000000 ) ) ;
#1548 = FACE_OUTER_BOUND ( 'NONE', #9863, .T. ) ;
#1549 = CARTESIAN_POINT ( 'NONE',  ( -0.4168742999989611953, -0.8811754754189499161, -0.1087450224342711852 ) ) ;
#1550 = DIRECTION ( 'NONE',  ( -1.000000000000000000, 0.000000000000000000, 0.000000000000000000 ) ) ;
#1551 = CARTESIAN_POINT ( 'NONE',  ( 0.2120693917185216271, -0.5839438448129662396, 0.2574819594177531479 ) ) ;
#1552 = CYLINDRICAL_SURFACE ( 'NONE', #2874, 0.4921259842519685179 ) ;
#1553 = CIRCLE ( 'NONE', #15987, 0.1181102362204718703 ) ;
#1554 = EDGE_LOOP ( 'NONE', ( #11117, #19270 ) ) ;
#1555 = CARTESIAN_POINT ( 'NONE',  ( 0.3122922550358837035, 0.3730863453234792848, 0.1075369453527844910 ) ) ;
#1556 = CIRCLE ( 'NONE', #7876, 0.01377952755905510404 ) ;
#1557 = EDGE_LOOP ( 'NONE', ( #14465, #20326, #18276, #7986 ) ) ;
#1558 = DIRECTION ( 'NONE',  ( 3.508908000000000588E-18, -0.4999999999999998890, -0.8660254037844388186 ) ) ;
#1559 = DIRECTION ( 'NONE',  ( 1.224646799147353207E-16, 1.000000000000000000, -0.000000000000000000 ) ) ;
#1560 = VERTEX_POINT ( 'NONE', #19724 ) ;
#1561 = CARTESIAN_POINT ( 'NONE',  ( 0.03532354024591839031, -0.6299212598425196763, -0.5531496062992127261 ) ) ;
#1562 = DIRECTION ( 'NONE',  ( 0.000000000000000000, 0.000000000000000000, 1.000000000000000000 ) ) ;
#1563 = CARTESIAN_POINT ( 'NONE',  ( -0.5335524835332333682, 0.1429116519061236767, 0.9202755905511811330 ) ) ;
#1564 = VERTEX_POINT ( 'NONE', #24234 ) ;
#1565 = EDGE_CURVE ( 'NONE', #2213, #15981, #2226, .T. ) ;
#1566 = DIRECTION ( 'NONE',  ( 0.000000000000000000, 0.000000000000000000, -1.000000000000000000 ) ) ;
#1567 = ORIENTED_EDGE ( 'NONE', *, *, #26156, .F. ) ;
#1568 = ADVANCED_FACE ( 'NONE', ( #2880 ), #4596, .F. ) ;
#1569 = DIRECTION ( 'NONE',  ( 0.000000000000000000, -1.000000000000000000, 0.000000000000000000 ) ) ;
#1570 = DIRECTION ( 'NONE',  ( 1.000000000000000000, 0.000000000000000000, 0.000000000000000000 ) ) ;
#1571 = CIRCLE ( 'NONE', #24136, 0.1771653543307086798 ) ;
#1572 = FACE_OUTER_BOUND ( 'NONE', #24833, .T. ) ;
#1573 = ORIENTED_EDGE ( 'NONE', *, *, #16459, .T. ) ;
#1574 = FACE_OUTER_BOUND ( 'NONE', #540, .T. ) ;
#1575 = CARTESIAN_POINT ( 'NONE',  ( -0.0006679551606482677165, 0.5322830454629158270, 0.3401574803149606252 ) ) ;
#1576 = CIRCLE ( 'NONE', #6546, 0.6212598425196850238 ) ;
#1577 = EDGE_LOOP ( 'NONE', ( #3628, #6530 ) ) ;
#1578 = CARTESIAN_POINT ( 'NONE',  ( 0.2041304421298449356, -0.2660793235464211093, 1.973425196850393970 ) ) ;
#1579 = CARTESIAN_POINT ( 'NONE',  ( -0.5708661417322835607, 0.000000000000000000, 0.000000000000000000 ) ) ;
#1580 = CARTESIAN_POINT ( 'NONE',  ( 0.5335524835332418059, -0.1429116519061131296, 0.9399606299212598381 ) ) ;
#1581 = FACE_OUTER_BOUND ( 'NONE', #21227, .T. ) ;
#1582 = VERTEX_POINT ( 'NONE', #514 ) ;
#1583 = CARTESIAN_POINT ( 'NONE',  ( -0.4055118110236220486, 4.966087413865251393E-17, 0.3425196850393700809 ) ) ;
#1584 = CIRCLE ( 'NONE', #6558, 0.4692913385826771866 ) ;
#1585 = CARTESIAN_POINT ( 'NONE',  ( -0.1771653543307086520, 0.000000000000000000, 0.000000000000000000 ) ) ;
#1586 = CARTESIAN_POINT ( 'NONE',  ( 0.4225410690757945842, 0.3242876858385722039, 1.747047244094488416 ) ) ;
#1587 = ORIENTED_EDGE ( 'NONE', *, *, #21256, .T. ) ;
#1588 = AXIS2_PLACEMENT_3D ( 'NONE', #21238, #19108, #17001 ) ;
#1589 = CARTESIAN_POINT ( 'NONE',  ( -0.06181127634704723650, -1.564461769117756029, 1.633858267716535639 ) ) ;
#1590 = CIRCLE ( 'NONE', #2500, 0.02362204724409448092 ) ;
#1591 = DIRECTION ( 'NONE',  ( 0.000000000000000000, 0.000000000000000000, 1.000000000000000000 ) ) ;
#1592 = CARTESIAN_POINT ( 'NONE',  ( 0.1516263115863346334, -0.4909405214979283838, 0.05579628926458630317 ) ) ;
#1593 = DIRECTION ( 'NONE',  ( 0.000000000000000000, 1.000000000000000000, 0.000000000000000000 ) ) ;
#1594 = ADVANCED_FACE ( 'NONE', ( #13215, #2743 ), #5009, .T. ) ;
#1595 = EDGE_LOOP ( 'NONE', ( #26419, #5301, #7926, #27061 ) ) ;
#1596 = CARTESIAN_POINT ( 'NONE',  ( -0.5609636804891235951, -0.5548708868579311781, 0.9753553170056504795 ) ) ;
#1597 = ORIENTED_EDGE ( 'NONE', *, *, #23655, .F. ) ;
#1598 = DIRECTION ( 'NONE',  ( 0.000000000000000000, -1.000000000000000000, 0.000000000000000000 ) ) ;
#1599 = CARTESIAN_POINT ( 'NONE',  ( -0.5622642684307268546, -0.5391005349161613891, -0.9826765462749343927 ) ) ;
#1600 = FACE_OUTER_BOUND ( 'NONE', #23729, .T. ) ;
#1601 = CARTESIAN_POINT ( 'NONE',  ( 0.3346456692913385988, 2.049113738730807321E-17, 1.973425196850393970 ) ) ;
#1602 = CARTESIAN_POINT ( 'NONE',  ( 0.7874015748031496509, -0.6060691875862913580, 0.08482860590294803715 ) ) ;
#1603 = ORIENTED_EDGE ( 'NONE', *, *, #23444, .F. ) ;
#1604 = AXIS2_PLACEMENT_3D ( 'NONE', #9998, #20742, #23148 ) ;
#1605 = DIRECTION ( 'NONE',  ( 1.000000000000000000, 0.000000000000000000, 0.000000000000000000 ) ) ;
#1606 = B_SPLINE_CURVE_WITH_KNOTS ( 'NONE', 3,
 ( #13341, #17306, #19706, #24214 ),
 .UNSPECIFIED., .F., .F.,
 ( 4, 4 ),
 ( 1.743059029969425078, 1.744705333033724992 ),
 .UNSPECIFIED. ) ;
#1607 = CARTESIAN_POINT ( 'NONE',  ( 0.3294268239828485600, 4.034315055438739563E-17, -0.1625845656552793450 ) ) ;
#1608 = EDGE_CURVE ( 'NONE', #17836, #10270, #11374, .T. ) ;
#1609 = CARTESIAN_POINT ( 'NONE',  ( 0.3102804211134971291, -0.1791085948260274507, -3.115157480314961091 ) ) ;
#1610 = CARTESIAN_POINT ( 'NONE',  ( 1.197070535079588716, 0.4724409448818898127, -1.078960298859116707 ) ) ;
#1611 = CARTESIAN_POINT ( 'NONE',  ( -0.03220957031754079214, -0.4921259842519684624, -1.569881889763779625 ) ) ;
#1612 = ORIENTED_EDGE ( 'NONE', *, *, #7598, .F. ) ;
#1613 = CARTESIAN_POINT ( 'NONE',  ( 0.4296318976989619842, -0.1458850421962461508, -1.934055118110236338 ) ) ;
#1614 = CIRCLE ( 'NONE', #25063, 0.3771653543307086909 ) ;
#1615 = SHAPE_REPRESENTATION ( 'Deep Groove Ball Bearing 20x37x9', ( #11588 ), #25599 ) ;
#1616 = CIRCLE ( 'NONE', #19678, 0.5905511811200284678 ) ;
#1617 = EDGE_LOOP ( 'NONE', ( #26636, #12625 ) ) ;
#1618 = CARTESIAN_POINT ( 'NONE',  ( -0.6002615430280354714, -0.1262890666645074822, -0.2459980689859385949 ) ) ;
#1619 = CARTESIAN_POINT ( 'NONE',  ( 0.5379714048901780288, 6.588249590315613132E-17, -0.2480314960629921295 ) ) ;
#1620 = CARTESIAN_POINT ( 'NONE',  ( 0.3242071728275122688, 0.4225965726692672564, 1.747047244094488194 ) ) ;
#1621 = ORIENTED_EDGE ( 'NONE', *, *, #19395, .F. ) ;
#1622 = ORIENTED_EDGE ( 'NONE', *, *, #6377, .T. ) ;
#1623 = ADVANCED_FACE ( 'NONE', ( #931 ), #12970, .T. ) ;
#1624 = PLANE ( 'NONE',  #18273 ) ;
#1625 = FACE_BOUND ( 'NONE', #12857, .T. ) ;
#1626 = B_SPLINE_CURVE_WITH_KNOTS ( 'NONE', 2,
 ( #5078, #9046, #11444 ),
 .UNSPECIFIED., .F., .F.,
 ( 3, 3 ),
 ( 0.000000000000000000, 1.000000000000000000 ),
 .UNSPECIFIED. ) ;
#1627 = CARTESIAN_POINT ( 'NONE',  ( 0.4446006764000813294, 0.02917857698668059607, -1.934055118110236560 ) ) ;
#1628 = EDGE_CURVE ( 'NONE', #9678, #24310, #22787, .T. ) ;
#1629 = CARTESIAN_POINT ( 'NONE',  ( -0.2817310484609168997, -0.2161381151963037983, 1.953740157480315043 ) ) ;
#1630 = ORIENTED_EDGE ( 'NONE', *, *, #18890, .F. ) ;
#1631 = EDGE_LOOP ( 'NONE', ( #23698, #24312, #24788, #16424 ) ) ;
#1632 = CARTESIAN_POINT ( 'NONE',  ( -0.6200889942125548115, -0.08218921327254806453, -0.2403616042849680556 ) ) ;
#1634 = CARTESIAN_POINT ( 'NONE',  ( -0.5708661417322835607, 0.000000000000000000, 0.9399606299212598381 ) ) ;
#1633 = CARTESIAN_POINT ( 'NONE',  ( -0.3010840436257778419, -0.2313841235333768398, -3.100567304031763172 ) ) ;
#1635 = VECTOR ( 'NONE', #4381, 39.37007874015748143 ) ;
#1636 = ORIENTED_EDGE ( 'NONE', *, *, #27592, .T. ) ;
#1637 = VERTEX_POINT ( 'NONE', #16323 ) ;
#1638 = VERTEX_POINT ( 'NONE', #14061 ) ;
#1639 = CARTESIAN_POINT ( 'NONE',  ( 0.6241887519799540485, -0.3029073140874564696, -0.5246508579836981490 ) ) ;
#1640 = DIRECTION ( 'NONE',  ( -0.1736481776669300814, 0.9848077530122080203, 0.000000000000000000 ) ) ;
#1641 = CIRCLE ( 'NONE', #24186, 0.01377952755905510404 ) ;
#1642 = CARTESIAN_POINT ( 'NONE',  ( -0.04679574315772200288, 0.3551931031211610357, -3.115157480314960647 ) ) ;
#1643 = CARTESIAN_POINT ( 'NONE',  ( -0.5511811023622047445, 3.375010863791918375E-17, 0.9202755905511811330 ) ) ;
#1644 = FACE_OUTER_BOUND ( 'NONE', #10088, .T. ) ;
#1645 = FACE_OUTER_BOUND ( 'NONE', #3746, .T. ) ;
#1646 = LINE ( 'NONE', #27513, #5048 ) ;
#1647 = B_SPLINE_CURVE_WITH_KNOTS ( 'NONE', 3,
 ( #2295, #10921, #26037, #9470, #11886, #5244 ),
 .UNSPECIFIED., .F., .F.,
 ( 4, 2, 4 ),
 ( 0.4045103800605749922, 0.4064350009536160102, 0.4083596218466570282 ),
 .UNSPECIFIED. ) ;
#1648 = CARTESIAN_POINT ( 'NONE',  ( 0.3191377210044040735, 0.3812612458998947962, 0.1140743250939253023 ) ) ;
#1649 = DIRECTION ( 'NONE',  ( 0.000000000000000000, 0.000000000000000000, 1.000000000000000000 ) ) ;
#1650 = ORIENTED_EDGE ( 'NONE', *, *, #22521, .F. ) ;
#1651 = CARTESIAN_POINT ( 'NONE',  ( 0.5417490723637030658, 0.1838434515542585190, 0.9399606299212597271 ) ) ;
#1652 = CARTESIAN_POINT ( 'NONE',  ( -0.3338887748335582772, -9.254566434645669797E-06, -2.341456692880161228 ) ) ;
#1653 = DIRECTION ( 'NONE',  ( 0.000000000000000000, 0.000000000000000000, -1.000000000000000000 ) ) ;
#1654 = FACE_OUTER_BOUND ( 'NONE', #1126, .T. ) ;
#1655 = CIRCLE ( 'NONE', #3429, 0.1771653543307086798 ) ;
#1656 = LINE ( 'NONE', #25670, #16003 ) ;
#1657 = PRODUCT_CONTEXT ( 'NONE', #12864, 'mechanical' ) ;
#1658 = DIRECTION ( 'NONE',  ( 0.000000000000000000, 0.000000000000000000, 1.000000000000000000 ) ) ;
#1659 = CARTESIAN_POINT ( 'NONE',  ( 0.2564944395515950104, 0.4441657790108120563, 1.747047244094488194 ) ) ;
#1660 = EDGE_LOOP ( 'NONE', ( #6013, #15520, #22967, #15519, #15320, #14141, #22628, #12183, #8642, #1327, #3586, #8439, #26231 ) ) ;
#1661 = AXIS2_PLACEMENT_3D ( 'NONE', #6156, #15392, #11060 ) ;
#1662 = ORIENTED_EDGE ( 'NONE', *, *, #10822, .F. ) ;
#1663 = DIRECTION ( 'NONE',  ( 1.000000000000000000, 0.000000000000000000, 0.000000000000000000 ) ) ;
#1664 = ORIENTED_EDGE ( 'NONE', *, *, #21562, .F. ) ;
#1665 = CARTESIAN_POINT ( 'NONE',  ( 0.2817828961649161412, -0.3666644560843326239, -1.928289503579156516 ) ) ;
#1666 = DIRECTION ( 'NONE',  ( 0.000000000000000000, -1.000000000000000000, 0.000000000000000000 ) ) ;
#1667 = ADVANCED_FACE ( 'NONE', ( #18269 ), #10473, .F. ) ;
#1668 = CARTESIAN_POINT ( 'NONE',  ( -0.3175540113612297932, -0.1078280746904006077, 1.973425196850393970 ) ) ;
#1669 = ORIENTED_EDGE ( 'NONE', *, *, #3115, .T. ) ;
#1670 = ORIENTED_EDGE ( 'NONE', *, *, #22246, .T. ) ;
#1671 = CARTESIAN_POINT ( 'NONE',  ( -0.03220957031754079214, -0.4921259842519685179, -1.550196850393700920 ) ) ;
#1672 = FACE_BOUND ( 'NONE', #15271, .T. ) ;
#1673 = VERTEX_POINT ( 'NONE', #23799 ) ;
#1674 = VERTEX_POINT ( 'NONE', #2446 ) ;
#1675 = DIRECTION ( 'NONE',  ( -0.000000000000000000, -0.000000000000000000, -1.000000000000000000 ) ) ;
#1676 = AXIS2_PLACEMENT_3D ( 'NONE', #17009, #8543, #17159 ) ;
#1677 = DIRECTION ( 'NONE',  ( 0.000000000000000000, 0.000000000000000000, -1.000000000000000000 ) ) ;
#1678 = CARTESIAN_POINT ( 'NONE',  ( 0.000000000000000000, 0.000000000000000000, -0.01377952755905511792 ) ) ;
#1679 = DIRECTION ( 'NONE',  ( 0.000000000000000000, 0.000000000000000000, 1.000000000000000000 ) ) ;
#1680 = CARTESIAN_POINT ( 'NONE',  ( -0.5385210225480960844, 0.4284847435812472183, 0.1322834645669291320 ) ) ;
#1681 = ( GEOMETRIC_REPRESENTATION_CONTEXT ( 3 ) GLOBAL_UNCERTAINTY_ASSIGNED_CONTEXT ( ( #1400 ) ) GLOBAL_UNIT_ASSIGNED_CONTEXT ( ( #650, #19998, #2884 ) ) REPRESENTATION_CONTEXT ( 'NONE', 'WORKASPACE' ) ) ;
#1682 = ORIENTED_EDGE ( 'NONE', *, *, #380, .T. ) ;
#1683 = CARTESIAN_POINT ( 'NONE',  ( 0.000000000000000000, 0.4232283464566928832, 0.2755905511811023723 ) ) ;
#1684 = CARTESIAN_POINT ( 'NONE',  ( 0.1490609433537086470, -0.2477132731973591961, 0.4096304796931519165 ) ) ;
#1685 = EDGE_CURVE ( 'NONE', #20128, #15627, #22080, .T. ) ;
#1686 = DIRECTION ( 'NONE',  ( -5.737213000000000442E-16, 1.000000000000000000, -1.224646799147353207E-16 ) ) ;
#1687 = DIRECTION ( 'NONE',  ( 0.000000000000000000, 0.000000000000000000, 1.000000000000000000 ) ) ;
#1688 = CARTESIAN_POINT ( 'NONE',  ( -0.4506204254121950470, -0.7490950376702004698, -0.003669893536069110569 ) ) ;
#1689 = CARTESIAN_POINT ( 'NONE',  ( 0.03008364706454716778, 0.1136516277932340530, -0.1968503937007874127 ) ) ;
#1690 = DIRECTION ( 'NONE',  ( 0.000000000000000000, 0.000000000000000000, -1.000000000000000000 ) ) ;
#1691 = CARTESIAN_POINT ( 'NONE',  ( 1.456051859513969730E-17, 0.5007874015748032814, 0.2574827755769819038 ) ) ;
#1692 = DIRECTION ( 'NONE',  ( 0.000000000000000000, -1.000000000000000000, 0.000000000000000000 ) ) ;
#1693 = EDGE_CURVE ( 'NONE', #27602, #16511, #21795, .T. ) ;
#1694 = EDGE_LOOP ( 'NONE', ( #4784, #800, #15232, #24470 ) ) ;
#1695 = CIRCLE ( 'NONE', #12060, 0.6212598425196850238 ) ;
#1696 = DIRECTION ( 'NONE',  ( -0.6698894744055998718, 0.000000000000000000, 0.7424608353849979636 ) ) ;
#1697 = CARTESIAN_POINT ( 'NONE',  ( 0.5241918773311228241, 6.419499047126015796E-17, -0.2342519685039370358 ) ) ;
#1698 = ORIENTED_EDGE ( 'NONE', *, *, #10194, .F. ) ;
#1699 = VERTEX_POINT ( 'NONE', #13055 ) ;
#1700 = CARTESIAN_POINT ( 'NONE',  ( -0.5085118447796470598, -0.06699507805605113553, -1.550196850393700920 ) ) ;
#1701 = DIRECTION ( 'NONE',  ( -0.9659258263664939337, -0.2588190448135644917, 0.000000000000000000 ) ) ;
#1702 = CARTESIAN_POINT ( 'NONE',  ( -0.5511811023622047445, 0.000000000000000000, 0.9202755905511811330 ) ) ;
#1703 = CARTESIAN_POINT ( 'NONE',  ( 0.4857053587577992437, 0.1648264847746080952, -1.550196850393700920 ) ) ;
#1704 = ORIENTED_EDGE ( 'NONE', *, *, #19694, .F. ) ;
#1705 = DIRECTION ( 'NONE',  ( 0.000000000000000000, 0.000000000000000000, 1.000000000000000000 ) ) ;
#1706 = FACE_OUTER_BOUND ( 'NONE', #25350, .T. ) ;
#1707 = AXIS2_PLACEMENT_3D ( 'NONE', #18329, #15682, #15955 ) ;
#1708 = EDGE_CURVE ( 'NONE', #2756, #15627, #3356, .T. ) ;
#1709 = CARTESIAN_POINT ( 'NONE',  ( -0.8725268807032540153, 0.000000000000000000, -0.2362204724409448231 ) ) ;
#1710 = CIRCLE ( 'NONE', #390, 0.09143349766193344108 ) ;
#1711 = ORIENTED_EDGE ( 'NONE', *, *, #11780, .F. ) ;
#1712 = CARTESIAN_POINT ( 'NONE',  ( 0.0002221395201541382898, 0.5322834645669292097, 0.1322810039474933141 ) ) ;
#1713 = ORIENTED_EDGE ( 'NONE', *, *, #14644, .F. ) ;
#1714 = CIRCLE ( 'NONE', #26498, 0.2395669291338582696 ) ;
#1715 = CARTESIAN_POINT ( 'NONE',  ( -0.1677079028045287967, 0.2904160862623510475, 1.953740157480315043 ) ) ;
#1716 = CARTESIAN_POINT ( 'NONE',  ( 0.3855916753034687172, 0.3382184156749162285, -1.550196850393700920 ) ) ;
#1717 = DIRECTION ( 'NONE',  ( -1.000000000000000000, 0.000000000000000000, 0.000000000000000000 ) ) ;
#1718 = EDGE_CURVE ( 'NONE', #4754, #27858, #20544, .T. ) ;
#1719 = CARTESIAN_POINT ( 'NONE',  ( -0.1429116519060979196, -0.5335524835332288163, 0.9399606299212598381 ) ) ;
#1720 = EDGE_CURVE ( 'NONE', #27077, #22659, #4736, .T. ) ;
#1721 = DIRECTION ( 'NONE',  ( 0.3420201433256691570, -0.9396926207859082059, 0.000000000000000000 ) ) ;
#1722 = ORIENTED_EDGE ( 'NONE', *, *, #4721, .T. ) ;
#1723 = CARTESIAN_POINT ( 'NONE',  ( 0.1525037638700915965, -0.2314035372547590119, 0.4381595109572582469 ) ) ;
#1724 = EDGE_CURVE ( 'NONE', #3938, #18589, #364, .T. ) ;
#1725 = ORIENTED_EDGE ( 'NONE', *, *, #4241, .T. ) ;
#1726 = ADVANCED_FACE ( 'NONE', ( #26317 ), #15603, .F. ) ;
#1727 = LINE ( 'NONE', #7814, #20994 ) ;
#1728 = AXIS2_PLACEMENT_3D ( 'NONE', #26105, #21872, #19190 ) ;
#1729 = ORIENTED_EDGE ( 'NONE', *, *, #3922, .F. ) ;
#1730 = AXIS2_PLACEMENT_3D ( 'NONE', #1173, #4976, #2977 ) ;
#1731 = CARTESIAN_POINT ( 'NONE',  ( 0.4856708409191126674, 0.1649135259639225026, -1.550196850393700920 ) ) ;
#1732 = CIRCLE ( 'NONE', #27448, 0.02362204724409448786 ) ;
#1733 = CARTESIAN_POINT ( 'NONE',  ( -1.357510822077637958, -1.563633646945708833, 1.633858267716535639 ) ) ;
#1734 = DIRECTION ( 'NONE',  ( 0.000000000000000000, 1.000000000000000000, 0.000000000000000000 ) ) ;
#1735 = VECTOR ( 'NONE', #24190, 39.37007874015748854 ) ;
#1736 = DIRECTION ( 'NONE',  ( 0.000000000000000000, 0.000000000000000000, -1.000000000000000000 ) ) ;
#1737 = ORIENTED_EDGE ( 'NONE', *, *, #24013, .T. ) ;
#1738 = CARTESIAN_POINT ( 'NONE',  ( -0.5616991426751372085, -0.5770957586701074282, 0.9615147744167586996 ) ) ;
#1739 = ORIENTED_EDGE ( 'NONE', *, *, #13974, .T. ) ;
#1740 = CARTESIAN_POINT ( 'NONE',  ( -0.6071192803969113205, -0.6030946203081917201, -0.9382345488190140248 ) ) ;
#1741 = AXIS2_PLACEMENT_3D ( 'NONE', #19071, #4646, #2125 ) ;
#1742 = CARTESIAN_POINT ( 'NONE',  ( 0.3543307086614173596, 0.000000000000000000, 1.953740157480315043 ) ) ;
#1743 = CARTESIAN_POINT ( 'NONE',  ( 1.197070535079588716, 0.07874015748031491790, 1.197070535079588716 ) ) ;
#1744 = DIRECTION ( 'NONE',  ( 1.000000000000000000, 0.000000000000000000, 0.000000000000000000 ) ) ;
#1745 = VERTEX_POINT ( 'NONE', #5410 ) ;
#1746 = DIRECTION ( 'NONE',  ( 0.000000000000000000, 0.000000000000000000, 1.000000000000000000 ) ) ;
#1747 = DIRECTION ( 'NONE',  ( 0.000000000000000000, -1.000000000000000000, 0.000000000000000000 ) ) ;
#1748 = ORIENTED_EDGE ( 'NONE', *, *, #22387, .F. ) ;
#1749 = CARTESIAN_POINT ( 'NONE',  ( -0.3392634445560575029, -0.1151354519024665318, -3.115157480314960647 ) ) ;
#1750 = UNCERTAINTY_MEASURE_WITH_UNIT (LENGTH_MEASURE( 1.000000000000000082E-05 ), #8720, 'distance_accuracy_value', 'NONE') ;
#1751 = CARTESIAN_POINT ( 'NONE',  ( -0.3599896729929590866, -0.2761764805255594313, -1.934055118110236338 ) ) ;
#1752 = ADVANCED_FACE ( 'NONE', ( #9783 ), #14715, .T. ) ;
#1753 = CIRCLE ( 'NONE', #25681, 0.5118110236220472231 ) ;
#1754 = EDGE_CURVE ( 'NONE', #4466, #3563, #22640, .T. ) ;
#1755 = VERTEX_POINT ( 'NONE', #9920 ) ;
#1756 = CARTESIAN_POINT ( 'NONE',  ( -0.5546128944410685380, -0.2284628647922791467, -0.2687227238212893665 ) ) ;
#1757 = CARTESIAN_POINT ( 'NONE',  ( -0.5144970376935736889, 0.1378076643338841389, 1.747047244094488194 ) ) ;
#1758 = VERTEX_POINT ( 'NONE', #20097 ) ;
#1759 = FACE_OUTER_BOUND ( 'NONE', #17673, .T. ) ;
#1760 = EDGE_LOOP ( 'NONE', ( #17994, #18349, #7720, #19973 ) ) ;
#1761 = CARTESIAN_POINT ( 'NONE',  ( 0.5925575908939920700, 0.000000000000000000, 0.000000000000000000 ) ) ;
#1762 = DIRECTION ( 'NONE',  ( 1.000000000000000000, 0.000000000000000000, 0.000000000000000000 ) ) ;
#1763 = FACE_OUTER_BOUND ( 'NONE', #3029, .T. ) ;
#1764 = DIRECTION ( 'NONE',  ( 0.000000000000000000, 1.000000000000000000, 0.000000000000000000 ) ) ;
#1765 = DIRECTION ( 'NONE',  ( 0.000000000000000000, 0.000000000000000000, -1.000000000000000000 ) ) ;
#1766 = ORIENTED_EDGE ( 'NONE', *, *, #4888, .T. ) ;
#1767 = CONICAL_SURFACE ( 'NONE', #12147, 0.6102362204724409711, 0.7853981625000032718 ) ;
#1768 = CARTESIAN_POINT ( 'NONE',  ( 0.3520466617656906050, 0.04638120790933070170, 1.953740157480315043 ) ) ;
#1769 = ADVANCED_FACE ( 'NONE', ( #16289 ), #13777, .F. ) ;
#1770 = ORIENTED_EDGE ( 'NONE', *, *, #6491, .F. ) ;
#1771 = PLANE ( 'NONE',  #16654 ) ;
#1772 = AXIS2_PLACEMENT_3D ( 'NONE', #26756, #16030, #5286 ) ;
#1773 = DIRECTION ( 'NONE',  ( 0.000000000000000000, 0.000000000000000000, 1.000000000000000000 ) ) ;
#1774 = AXIS2_PLACEMENT_3D ( 'NONE', #6050, #23287, #16772 ) ;
#1775 = EDGE_LOOP ( 'NONE', ( #13680, #19313, #6854, #316, #10783, #6020, #16688, #25651, #23336, #23483, #140, #14286, #18043 ) ) ;
#1776 = EDGE_LOOP ( 'NONE', ( #5191, #3229 ) ) ;
#1777 = CARTESIAN_POINT ( 'NONE',  ( 2.632951206231566310, -0.4724409448818898127, 0.6874452634183660926 ) ) ;
#1778 = CARTESIAN_POINT ( 'NONE',  ( -0.2602238532265429005, 0.000000000000000000, -0.2362204724409449064 ) ) ;
#1779 = CARTESIAN_POINT ( 'NONE',  ( -0.2693339498142344746, -0.2362439534887506021, -3.115157480314960647 ) ) ;
#1780 = CARTESIAN_POINT ( 'NONE',  ( -0.4842519685039370358, 0.000000000000000000, -0.2480314960629921295 ) ) ;
#1781 = DIRECTION ( 'NONE',  ( 0.000000000000000000, 0.000000000000000000, -1.000000000000000000 ) ) ;
#1782 = CARTESIAN_POINT ( 'NONE',  ( 0.6117062799105453808, 0.1085321106658576895, 0.09685039370078740717 ) ) ;
#1783 = DIRECTION ( 'NONE',  ( 0.000000000000000000, -1.000000000000000000, 0.000000000000000000 ) ) ;
#1784 = ADVANCED_FACE ( 'NONE', ( #7526, #1180 ), #25038, .T. ) ;
#1785 = CARTESIAN_POINT ( 'NONE',  ( -0.09586345242798390009, 0.2165354330708661734, -3.246875208232354648 ) ) ;
#1786 = EDGE_CURVE ( 'NONE', #3563, #16499, #2562, .T. ) ;
#1787 = DIRECTION ( 'NONE',  ( 0.000000000000000000, 1.000000000000000000, 0.000000000000000000 ) ) ;
#1788 = EDGE_CURVE ( 'NONE', #6256, #18898, #12424, .T. ) ;
#1789 = AXIS2_PLACEMENT_3D ( 'NONE', #2792, #20182, #20047 ) ;
#1790 = ORIENTED_EDGE ( 'NONE', *, *, #19478, .T. ) ;
#1791 = CARTESIAN_POINT ( 'NONE',  ( 0.1490609433615242285, -0.4786070381542913421, 5.861244094488189820E-17 ) ) ;
#1792 = DIRECTION ( 'NONE',  ( -1.000000000000000000, -1.224646799147356165E-16, 0.000000000000000000 ) ) ;
#1793 = FACE_OUTER_BOUND ( 'NONE', #6745, .T. ) ;
#1794 = AXIS2_PLACEMENT_3D ( 'NONE', #3332, #8026, #8807 ) ;
#1795 = ORIENTED_EDGE ( 'NONE', *, *, #27521, .F. ) ;
#1796 = CARTESIAN_POINT ( 'NONE',  ( -0.7434700980050995556, 0.5844848647591116553, -0.4795863528207047755 ) ) ;
#1797 = ( LENGTH_UNIT ( ) NAMED_UNIT ( * ) SI_UNIT ( $, .METRE. ) ) ;
#1798 = CARTESIAN_POINT ( 'NONE',  ( -0.3019498226894488102, 0.3592501948414881796, 0.07637630773773090853 ) ) ;
#1799 = DIRECTION ( 'NONE',  ( 0.000000000000000000, 0.000000000000000000, 1.000000000000000000 ) ) ;
#1800 = EDGE_CURVE ( 'NONE', #5887, #6621, #23801, .T. ) ;
#1801 = EDGE_LOOP ( 'NONE', ( #9800, #18373 ) ) ;
#1802 = VERTEX_POINT ( 'NONE', #20523 ) ;
#1803 = CARTESIAN_POINT ( 'NONE',  ( 0.3213305936751376102, 0.1584254766472200371, -3.115157480314960647 ) ) ;
#1804 = VERTEX_POINT ( 'NONE', #3547 ) ;
#1805 = CARTESIAN_POINT ( 'NONE',  ( -0.1200170377978880404, -0.4465874321618643061, -1.928289503579156294 ) ) ;
#1806 = VERTEX_POINT ( 'NONE', #5550 ) ;
#1807 = CARTESIAN_POINT ( 'NONE',  ( 0.6889763779527560139, 8.437527159479796553E-17, -0.2618110236220472231 ) ) ;
#1808 = CARTESIAN_POINT ( 'NONE',  ( -0.1078280746904014958, -0.3175540113612295157, 1.973425196850393970 ) ) ;
#1809 = EDGE_CURVE ( 'NONE', #18324, #3673, #7442, .T. ) ;
#1810 = ORIENTED_EDGE ( 'NONE', *, *, #27252, .F. ) ;
#1811 = ORIENTED_EDGE ( 'NONE', *, *, #169, .T. ) ;
#1812 = CARTESIAN_POINT ( 'NONE',  ( -0.3252100150720461658, 0.3707612262532960501, -1.550196850393700920 ) ) ;
#1813 = FACE_BOUND ( 'NONE', #23770, .T. ) ;
#1814 = ORIENTED_EDGE ( 'NONE', *, *, #967, .F. ) ;
#1815 = EDGE_LOOP ( 'NONE', ( #12372, #8684, #25819, #8751 ) ) ;
#1816 = AXIS2_PLACEMENT_3D ( 'NONE', #10489, #25619, #21244 ) ;
#1817 = AXIS2_PLACEMENT_3D ( 'NONE', #6481, #17216, #21462 ) ;
#1818 = ITEM_DEFINED_TRANSFORMATION ( 'NONE', 'NONE', #12485,  #11588 ) ;
#1819 = CARTESIAN_POINT ( 'NONE',  ( 0.000000000000000000, 0.000000000000000000, 0.1992125984251968684 ) ) ;
#1820 = CYLINDRICAL_SURFACE ( 'NONE', #15991, 0.1181102362204718703 ) ;
#1821 = ORIENTED_EDGE ( 'NONE', *, *, #19932, .F. ) ;
#1822 = CIRCLE ( 'NONE', #7231, 0.1003956692913385990 ) ;
#1823 = B_SPLINE_CURVE_WITH_KNOTS ( 'NONE', 3,
 ( #1040, #3129, #9631, #18236, #26446, #7110 ),
 .UNSPECIFIED., .F., .F.,
 ( 4, 2, 4 ),
 ( 0.9031406754215579591, 0.9046454396443710522, 0.9061502038671850334 ),
 .UNSPECIFIED. ) ;
#1824 = ORIENTED_EDGE ( 'NONE', *, *, #3257, .F. ) ;
#1825 = PLANE ( 'NONE',  #7840 ) ;
#1826 = EDGE_CURVE ( 'NONE', #17190, #19458, #11615, .T. ) ;
#1827 = FACE_OUTER_BOUND ( 'NONE', #23500, .T. ) ;
#1828 = CARTESIAN_POINT ( 'NONE',  ( 0.03937007874015747977, 0.000000000000000000, -0.3740157480314960647 ) ) ;
#1829 = DIRECTION ( 'NONE',  ( -0.7071067811865470176, -0.7071067811865480168, 0.000000000000000000 ) ) ;
#1830 = ADVANCED_FACE ( 'NONE', ( #7380 ), #27323, .F. ) ;
#1831 = CARTESIAN_POINT ( 'NONE',  ( -0.6054712446264385317, -0.1811734661067123109, 0.2234263948845375547 ) ) ;
#1832 = DIRECTION ( 'NONE',  ( -0.9930684569432060016, -0.1175373975568611284, 1.439417707043116609E-17 ) ) ;
#1833 = LINE ( 'NONE', #12286, #667 ) ;
#1834 = CARTESIAN_POINT ( 'NONE',  ( -2.685748425196850164E-17, 0.000000000000000000, -3.115157480314960647 ) ) ;
#1835 = CIRCLE ( 'NONE', #17621, 0.8163976377952757435 ) ;
#1836 = DIRECTION ( 'NONE',  ( 1.000000000000000000, 0.000000000000000000, 0.000000000000000000 ) ) ;
#1837 = ORIENTED_EDGE ( 'NONE', *, *, #5197, .F. ) ;
#1838 = FACE_OUTER_BOUND ( 'NONE', #26109, .T. ) ;
#1839 = LENGTH_MEASURE_WITH_UNIT ( LENGTH_MEASURE( 0.02539999999999999897 ), #25850 ) ;
#1840 = ORIENTED_EDGE ( 'NONE', *, *, #26753, .F. ) ;
#1841 = CIRCLE ( 'NONE', #24842, 0.5531496062992126150 ) ;
#1842 = LINE ( 'NONE', #25717, #22886 ) ;
#1843 = DIRECTION ( 'NONE',  ( 0.000000000000000000, 0.000000000000000000, 1.000000000000000000 ) ) ;
#1844 = CARTESIAN_POINT ( 'NONE',  ( -0.3062557396300204515, -0.6341756901046630146, 0.1443310008627645136 ) ) ;
#1845 = DIRECTION ( 'NONE',  ( 0.000000000000000000, -1.000000000000000000, 0.000000000000000000 ) ) ;
#1846 = ORIENTED_EDGE ( 'NONE', *, *, #19267, .F. ) ;
#1847 = DIRECTION ( 'NONE',  ( -1.000000000000000000, 1.224646799147353454E-16, 0.000000000000000000 ) ) ;
#1848 = EDGE_LOOP ( 'NONE', ( #13711, #22030, #20883, #10591 ) ) ;
#1849 = ORIENTED_EDGE ( 'NONE', *, *, #8001, .T. ) ;
#1850 = EDGE_CURVE ( 'NONE', #14002, #24185, #9702, .T. ) ;
#1851 = SURFACE_STYLE_FILL_AREA ( #5675 ) ;
#1852 = CARTESIAN_POINT ( 'NONE',  ( 0.4690668203917182089, 0.08212126673940543797, 0.2330651858111663088 ) ) ;
#1853 = LINE ( 'NONE', #23488, #2325 ) ;
#1854 = VECTOR ( 'NONE', #10953, 39.37007874015748854 ) ;
#1855 = DIRECTION ( 'NONE',  ( -1.000000000000000000, 0.000000000000000000, 0.000000000000000000 ) ) ;
#1856 = ORIENTED_EDGE ( 'NONE', *, *, #775, .F. ) ;
#1857 = DIRECTION ( 'NONE',  ( 0.3420201433256691015, -0.9396926207859082059, 0.000000000000000000 ) ) ;
#1858 = CARTESIAN_POINT ( 'NONE',  ( -0.07874015748031495954, 0.1968503937007873850, -3.272637795275590733 ) ) ;
#1859 = ORIENTED_EDGE ( 'NONE', *, *, #22214, .F. ) ;
#1860 = CARTESIAN_POINT ( 'NONE',  ( 0.1482986320106470801, -0.3007905576423859917, 1.973425196850393970 ) ) ;
#1861 = DIRECTION ( 'NONE',  ( -0.000000000000000000, -0.000000000000000000, 1.000000000000000000 ) ) ;
#1862 = CARTESIAN_POINT ( 'NONE',  ( 0.0005696707463081691122, 0.4606295689977897845, 0.1903859677794648431 ) ) ;
#1863 = CIRCLE ( 'NONE', #3660, 0.4811133748141622202 ) ;
#1864 = CIRCLE ( 'NONE', #3209, 0.1181102362204718703 ) ;
#1865 = CARTESIAN_POINT ( 'NONE',  ( 0.4783323773986630778, -0.2762247810518744240, 0.9399606299212598381 ) ) ;
#1866 = CARTESIAN_POINT ( 'NONE',  ( 0.003937007874015826907, -4.393043307086613241E-18, 0.000000000000000000 ) ) ;
#1867 = VERTEX_POINT ( 'NONE', #26724 ) ;
#1868 = CARTESIAN_POINT ( 'NONE',  ( 0.2693781226336498524, 0.2362017869178958951, -3.115157480314961980 ) ) ;
#1869 = VERTEX_POINT ( 'NONE', #16006 ) ;
#1870 = ORIENTED_EDGE ( 'NONE', *, *, #765, .F. ) ;
#1871 = AXIS2_PLACEMENT_3D ( 'NONE', #22035, #21385, #11297 ) ;
#1872 = CARTESIAN_POINT ( 'NONE',  ( -0.2268096725200260955, 0.4600326175569864340, -1.550196850393700920 ) ) ;
#1873 = CYLINDRICAL_SURFACE ( 'NONE', #17851, 0.2395669291338582696 ) ;
#1874 = DIRECTION ( 'NONE',  ( 0.6234898018587330393, -0.7818314824680302477, 0.000000000000000000 ) ) ;
#1875 = CARTESIAN_POINT ( 'NONE',  ( -0.4225410690760224575, -0.3242876858381196770, 1.747047244094488194 ) ) ;
#1876 = EDGE_CURVE ( 'NONE', #10634, #15096, #5263, .T. ) ;
#1877 = DIRECTION ( 'NONE',  ( 0.000000000000000000, 0.000000000000000000, 1.000000000000000000 ) ) ;
#1878 = ORIENTED_EDGE ( 'NONE', *, *, #21317, .T. ) ;
#1879 = AXIS2_PLACEMENT_3D ( 'NONE', #19649, #10746, #6792 ) ;
#1880 = AXIS2_PLACEMENT_3D ( 'NONE', #20412, #18117, #5296 ) ;
#1881 = CARTESIAN_POINT ( 'NONE',  ( -0.6138531223217379429, -0.4891464190266830436, -0.9948699164928014316 ) ) ;
#1882 = PRODUCT_DEFINITION ( 'UNKNOWN', '', #26496, #17018 ) ;
#1883 = DIRECTION ( 'NONE',  ( 1.000000000000000000, 0.000000000000000000, 0.000000000000000000 ) ) ;
#1884 = CARTESIAN_POINT ( 'NONE',  ( 0.07874015748031489015, 9.642888182262615344E-18, -0.3779527559055118058 ) ) ;
#1885 = CARTESIAN_POINT ( 'NONE',  ( -6.132876883919029269E-17, -0.5007874015748031704, 0.3059055118110236560 ) ) ;
#1886 = EDGE_CURVE ( 'NONE', #7494, #4592, #5665, .T. ) ;
#1887 = ORIENTED_EDGE ( 'NONE', *, *, #14871, .F. ) ;
#1888 = LINE ( 'NONE', #27610, #24730 ) ;
#1889 = EDGE_CURVE ( 'NONE', #18210, #12438, #181, .T. ) ;
#1890 = ORIENTED_EDGE ( 'NONE', *, *, #2911, .F. ) ;
#1891 = FACE_OUTER_BOUND ( 'NONE', #4069, .T. ) ;
#1892 = CARTESIAN_POINT ( 'NONE',  ( -0.4585215200179055817, 0.03001016326912889221, -1.928289503579156516 ) ) ;
#1893 = CIRCLE ( 'NONE', #7287, 0.09143349766193344108 ) ;
#1894 = DIRECTION ( 'NONE',  ( 0.000000000000000000, -1.000000000000000000, 0.000000000000000000 ) ) ;
#1895 = COLOUR_RGB ( '', 0.40784314, 0.44705882, 0.49803922) ;
#1896 = ORIENTED_EDGE ( 'NONE', *, *, #10087, .F. ) ;
#1897 = ORIENTED_EDGE ( 'NONE', *, *, #23990, .F. ) ;
#1898 = CARTESIAN_POINT ( 'NONE',  ( -0.4881018399981850719, -0.4577461864050251794, -0.1927445091220988116 ) ) ;
#1899 = SURFACE_SIDE_STYLE ('',( #20830 ) ) ;
#1900 = ORIENTED_EDGE ( 'NONE', *, *, #17550, .F. ) ;
#1901 = CARTESIAN_POINT ( 'NONE',  ( -0.6708784387195235732, -0.1533826961018689150, 0.3401599409343967761 ) ) ;
#1902 = CARTESIAN_POINT ( 'NONE',  ( -0.6086685665488132946, -0.5056997808540499850, 0.9923580223642571863 ) ) ;
#1903 = DIRECTION ( 'NONE',  ( 0.000000000000000000, 0.000000000000000000, -1.000000000000000000 ) ) ;
#1904 = B_SPLINE_SURFACE_WITH_KNOTS ( 'NONE', 3, 3, ( 
 ( #4850, #11356, #19838, #9087 ),
 ( #13465, #19569, #6573, #15614 ),
 ( #19703, #17579, #628, #22090 ),
 ( #21544, #17302, #2722, #15199 ),
 ( #15479, #19423, #21823, #24075 ),
 ( #10945, #2458, #26328, #6714 ),
 ( #23810, #2316, #25784, #4580 ),
 ( #4715, #19972, #6991, #15068 ),
 ( #11213, #23678, #11085, #4313 ),
 ( #115, #12918, #2189, #10807 ),
 ( #371, #4452, #8686, #26192 ),
 ( #23944, #6850, #250, #8821 ),
 ( #17437, #11491, #17837, #7390 ) ),
 .UNSPECIFIED., .F., .F., .F.,
 ( 4, 1, 1, 1, 1, 1, 1, 1, 1, 1, 4 ),
 ( 4, 4 ),
 ( 0.3833360769390280476, 0.3893635454205919832, 0.3944867497131970269, 0.4047331582984080023, 0.4098563625910129904, 0.4201027711762239658, 0.4252259754688289539, 0.4405955883466449730, 0.4508419969318550047, 0.4713348141022760118, 0.4911627496483090272 ),
 ( -0.5999999999999999778, 0.5999999999999999778 ),
 .UNSPECIFIED. ) ;
#1905 = CARTESIAN_POINT ( 'NONE',  ( -0.3013593406941685315, 0.3597456680659448791, 0.1992142434433716580 ) ) ;
#1906 = EDGE_CURVE ( 'NONE', #25174, #23007, #23999, .T. ) ;
#1907 = ORIENTED_EDGE ( 'NONE', *, *, #6203, .F. ) ;
#1908 = AXIS2_PLACEMENT_3D ( 'NONE', #8443, #25400, #25959 ) ;
#1909 = CARTESIAN_POINT ( 'NONE',  ( -0.3520466617656973218, 0.04638120790932954290, 1.953740157480315043 ) ) ;
#1910 = EDGE_LOOP ( 'NONE', ( #18795, #3060, #19622, #12675 ) ) ;
#1911 = EDGE_CURVE ( 'NONE', #1674, #11878, #18256, .T. ) ;
#1912 = DIRECTION ( 'NONE',  ( 1.000000000000000000, 0.000000000000000000, 0.000000000000000000 ) ) ;
#1914 = CARTESIAN_POINT ( 'NONE',  ( 0.5671862884095085766, -0.07472527936312026164, 0.9399606299212598381 ) ) ;
#1913 = CARTESIAN_POINT ( 'NONE',  ( 0.0003854097504292619937, 0.4692912202195575477, 0.1992142434433716580 ) ) ;
#1915 = ORIENTED_EDGE ( 'NONE', *, *, #329, .T. ) ;
#1916 = ORIENTED_EDGE ( 'NONE', *, *, #5024, .F. ) ;
#1917 = LINE ( 'NONE', #25369, #23538 ) ;
#1918 = DIRECTION ( 'NONE',  ( -1.000000000000000000, 0.000000000000000000, 0.000000000000000000 ) ) ;
#1919 = ADVANCED_FACE ( 'NONE', ( #21749 ), #8460, .T. ) ;
#1921 = CARTESIAN_POINT ( 'NONE',  ( -0.02438677169350859236, -0.3726024258163779246, -3.115157480314960647 ) ) ;
#1922 = EDGE_CURVE ( 'NONE', #11128, #20567, #12440, .T. ) ;
#1923 = DIRECTION ( 'NONE',  ( 0.000000000000000000, 0.000000000000000000, 1.000000000000000000 ) ) ;
#1924 = DIRECTION ( 'NONE',  ( -1.224646799147353207E-16, 1.000000000000000000, 0.000000000000000000 ) ) ;
#1925 = DIRECTION ( 'NONE',  ( -1.000000000000000000, 0.000000000000000000, 0.000000000000000000 ) ) ;
#1926 = DIRECTION ( 'NONE',  ( 1.000000000000000000, 0.000000000000000000, 0.000000000000000000 ) ) ;
#1927 = CARTESIAN_POINT ( 'NONE',  ( 0.4793172621399190980, -0.1288129352161812291, -1.569881889763779625 ) ) ;
#1928 = CARTESIAN_POINT ( 'NONE',  ( -0.7171569026305500971, -0.1628805401855070167, 0.2763636194294596948 ) ) ;
#1929 = CARTESIAN_POINT ( 'NONE',  ( -0.4382482975805018222, 0.3362148458988871713, 0.9202755905511811330 ) ) ;
#1930 = AXIS2_PLACEMENT_3D ( 'NONE', #8276, #16896, #4038 ) ;
#1931 = ADVANCED_FACE ( 'NONE', ( #21885, #3056 ), #18165, .T. ) ;
#1932 = CARTESIAN_POINT ( 'NONE',  ( 0.5525886237723619532, 0.1481199686341792554, 0.9399606299212597271 ) ) ;
#1933 = AXIS2_PLACEMENT_3D ( 'NONE', #3288, #11638, #1202 ) ;
#1934 = VERTEX_POINT ( 'NONE', #24403 ) ;
#1935 = VERTEX_POINT ( 'NONE', #20033 ) ;
#1936 = CARTESIAN_POINT ( 'NONE',  ( 0.000000000000000000, 0.000000000000000000, 0.2637795275590551491 ) ) ;
#1937 = CARTESIAN_POINT ( 'NONE',  ( -0.2564944395515745823, 0.4441657790107744752, 1.766732283464566899 ) ) ;
#1938 = EDGE_LOOP ( 'NONE', ( #18405, #23530, #16825, #17076 ) ) ;
#1939 = AXIS2_PLACEMENT_3D ( 'NONE', #16280, #5401, #14020 ) ;
#1940 = EDGE_LOOP ( 'NONE', ( #3671, #24447, #23194, #8528 ) ) ;
#1941 = CARTESIAN_POINT ( 'NONE',  ( -0.3102476824511484210, -0.1791601451668926870, -3.115157480314960647 ) ) ;
#1942 = VERTEX_POINT ( 'NONE', #2521 ) ;
#1943 = FACE_OUTER_BOUND ( 'NONE', #20847, .T. ) ;
#1944 = CARTESIAN_POINT ( 'NONE',  ( 0.006151574803149606648, -1.315836188112322458E-17, 0.1074461786882927178 ) ) ;
#1945 = CARTESIAN_POINT ( 'NONE',  ( -0.08676778863011193332, -0.3239425792934405024, 1.973425196850393970 ) ) ;
#1946 = EDGE_LOOP ( 'NONE', ( #5707, #22229, #3948, #19794, #660, #9639 ) ) ;
#1947 = ORIENTED_EDGE ( 'NONE', *, *, #9292, .F. ) ;
#1948 = EDGE_CURVE ( 'NONE', #14897, #8484, #427, .T. ) ;
#1949 = LINE ( 'NONE', #23449, #13384 ) ;
#1950 = CARTESIAN_POINT ( 'NONE',  ( -0.3714054139060130044, 0.06566393819133267695, 0.1992150590373740204 ) ) ;
#1951 = VERTEX_POINT ( 'NONE', #18020 ) ;
#1952 = VERTEX_POINT ( 'NONE', #2654 ) ;
#1953 = ORIENTED_EDGE ( 'NONE', *, *, #18523, .F. ) ;
#1954 = CARTESIAN_POINT ( 'NONE',  ( -0.1669771619560911358, -0.4570419016575711368, 0.1827409795183129182 ) ) ;
#1955 = ADVANCED_FACE ( 'NONE', ( #11280 ), #971, .T. ) ;
#1956 = AXIS2_PLACEMENT_3D ( 'NONE', #9250, #22687, #14227 ) ;
#1957 = ( BOUNDED_CURVE ( )  B_SPLINE_CURVE ( 2, ( #3595, #27346, #24646 ),
 .UNSPECIFIED., .F., .T. ) 
 B_SPLINE_CURVE_WITH_KNOTS ( ( 3, 3 ),
 ( 0.000000000000000000, 0.5842180690389598974 ),
 .UNSPECIFIED. ) 
 CURVE ( )  GEOMETRIC_REPRESENTATION_ITEM ( )  RATIONAL_B_SPLINE_CURVE ( ( 1.000000000000000000, 1.154700538379251906, 1.000000000000000000 ) ) 
 REPRESENTATION_ITEM ( '' )  ) ;
#1958 = TOROIDAL_SURFACE ( 'NONE', #5096, 0.5610236220472440971, 0.1003937007874015908 ) ;
#1959 = CARTESIAN_POINT ( 'NONE',  ( 0.0005114926878485707464, 0.3662580330841583853, 0.08455817587929100043 ) ) ;
#1960 = CARTESIAN_POINT ( 'NONE',  ( -0.01308409974552196542, 0.3147525462474320412, -3.645993128380378590 ) ) ;
#1961 = CARTESIAN_POINT ( 'NONE',  ( 0.4895436826821757959, 0.08692528595281577564, 0.1615162260900951940 ) ) ;
#1962 = ORIENTED_EDGE ( 'NONE', *, *, #1502, .T. ) ;
#1963 = CARTESIAN_POINT ( 'NONE',  ( -0.6711032387266614441, -0.1523958994813200962, 0.1322834645669291320 ) ) ;
#1964 = CIRCLE ( 'NONE', #24961, 0.4055118110236220486 ) ;
#1965 = CARTESIAN_POINT ( 'NONE',  ( -1.928513779527558736E-17, 0.000000000000000000, -0.4566929133858267376 ) ) ;
#1966 = DIRECTION ( 'NONE',  ( 0.000000000000000000, 0.000000000000000000, 1.000000000000000000 ) ) ;
#1967 = CARTESIAN_POINT ( 'NONE',  ( -0.4413253306211258331, -0.7852380862899401848, -0.03056779453504937169 ) ) ;
#1968 = CARTESIAN_POINT ( 'NONE',  ( -0.6299212598425196763, -0.4724409448818898127, 0.6411263657805708061 ) ) ;
#1969 = DIRECTION ( 'NONE',  ( 0.000000000000000000, 1.000000000000000000, 0.000000000000000000 ) ) ;
#1970 = FACE_BOUND ( 'NONE', #21845, .T. ) ;
#1971 = CLOSED_SHELL ( 'NONE', ( #15948, #15056, #8958, #16202, #10885, #14911, #6900, #2595, #9142, #9759, #11797, #21604, #23526, #3346, #19780, #1160, #17922, #5843, #15313, #9809, #10332, #20220, #565, #12662, #11099, #23134, #1162, #26300, #20891, #109, #23751, #26904, #15516, #491, #12592, #16279, #12320, #22712, #12212, #21149, #4868, #10021, #11378, #13614, #8619, #10786, #4999, #11411, #19167, #7508, #16182, #21953, #18937, #16308, #1931, #10879, #21976, #24048, #23772, #7397, #25804, #17407 ) ) ;
#1972 = CARTESIAN_POINT ( 'NONE',  ( 0.06048688226685065145, 0.2165354330708661457, -3.193930429277373140 ) ) ;
#1973 = EDGE_LOOP ( 'NONE', ( #20423, #21873, #19738, #3498, #20930 ) ) ;
#1974 = CARTESIAN_POINT ( 'NONE',  ( 0.3119936278842271316, -0.6460736482368880651, 0.3122824329307916646 ) ) ;
#1975 = CARTESIAN_POINT ( 'NONE',  ( 0.1285103288269283661, -0.3545966721392122545, 0.07637795275590551769 ) ) ;
#1976 = ORIENTED_EDGE ( 'NONE', *, *, #15552, .T. ) ;
#1977 = AXIS2_PLACEMENT_3D ( 'NONE', #6220, #4092, #12279 ) ;
#1978 = SPHERICAL_SURFACE ( 'NONE', #5233, 0.1299232283464566984 ) ;
#1979 = DIRECTION ( 'NONE',  ( 1.000000000000000000, 0.000000000000000000, 0.000000000000000000 ) ) ;
#1980 = AXIS2_PLACEMENT_3D ( 'NONE', #7829, #5567, #26603 ) ;
#1981 = CARTESIAN_POINT ( 'NONE',  ( 0.1775991818008376133, 0.5230301363771421297, 0.9202755905511811330 ) ) ;
#1982 = ORIENTED_EDGE ( 'NONE', *, *, #10724, .T. ) ;
#1983 = EDGE_CURVE ( 'NONE', #26656, #2802, #10615, .T. ) ;
#1984 = CARTESIAN_POINT ( 'NONE',  ( -0.6562077975700374433, -2.731848031496062854E-17, 0.07874015748031495954 ) ) ;
#1985 = ORIENTED_EDGE ( 'NONE', *, *, #5181, .T. ) ;
#1986 = DIRECTION ( 'NONE',  ( 0.000000000000000000, 0.000000000000000000, -1.000000000000000000 ) ) ;
#1987 = CARTESIAN_POINT ( 'NONE',  ( -0.4932821129636645874, 0.08637579872942342807, 0.2574803149606298969 ) ) ;
#1988 = CARTESIAN_POINT ( 'NONE',  ( -0.3998447049182496382, 0.4754871227240771714, 0.09685039370078740717 ) ) ;
#1989 = CARTESIAN_POINT ( 'NONE',  ( -0.6299212598425196763, -1.092519685074702762, 0.000000000000000000 ) ) ;
#1990 = AXIS2_PLACEMENT_3D ( 'NONE', #5836, #3689, #3843 ) ;
#1991 = ORIENTED_EDGE ( 'NONE', *, *, #20752, .T. ) ;
#1992 = CYLINDRICAL_SURFACE ( 'NONE', #10340, 0.1771653543307086798 ) ;
#1993 = DIRECTION ( 'NONE',  ( -0.8660254037844388186, -0.4999999999999997780, 0.000000000000000000 ) ) ;
#1994 = CARTESIAN_POINT ( 'NONE',  ( 0.4897507849252922818, 0.08575075074490855209, 0.1140743250802734171 ) ) ;
#1995 = ORIENTED_EDGE ( 'NONE', *, *, #12248, .F. ) ;
#1996 = CARTESIAN_POINT ( 'NONE',  ( 0.3346456692913385988, 0.000000000000000000, 1.973425196850393970 ) ) ;
#1997 = CARTESIAN_POINT ( 'NONE',  ( 0.000000000000000000, 0.000000000000000000, 0.2362204724409449064 ) ) ;
#1998 = DIRECTION ( 'NONE',  ( -0.9790454724845842893, -0.1018208755700880375, -0.1763589297585410332 ) ) ;
#1999 = VECTOR ( 'NONE', #24433, 39.37007874015748854 ) ;
#2000 = CARTESIAN_POINT ( 'NONE',  ( -0.2442565704126459791, -0.4954197419817803483, 0.9399606299212598381 ) ) ;
#2001 = VECTOR ( 'NONE', #27161, 39.37007874015748143 ) ;
#2002 = CARTESIAN_POINT ( 'NONE',  ( -6.092417322834646079E-17, 0.5905905511811023745, -3.272637795275590733 ) ) ;
#2003 = ORIENTED_EDGE ( 'NONE', *, *, #14808, .T. ) ;
#2004 = DIRECTION ( 'NONE',  ( -0.000000000000000000, 1.000000000000000000, 0.000000000000000000 ) ) ;
#2005 = VERTEX_POINT ( 'NONE', #5050 ) ;
#2006 = CARTESIAN_POINT ( 'NONE',  ( -0.2066929133858267931, 0.6299212598425196763, 0.000000000000000000 ) ) ;
#2007 = CIRCLE ( 'NONE', #5137, 0.3149606299212598381 ) ;
#2008 = VERTEX_POINT ( 'NONE', #16083 ) ;
#2009 = CARTESIAN_POINT ( 'NONE',  ( 0.1327036767636011194, 0.4954415918535620689, -1.550196850393700920 ) ) ;
#2010 = CARTESIAN_POINT ( 'NONE',  ( -0.2530774914999985303, -0.5130713940403577311, 0.9399606299212601712 ) ) ;
#2011 = CARTESIAN_POINT ( 'NONE',  ( 0.1189624676717049440, -0.3253923344978161825, 0.1377952755905510474 ) ) ;
#2012 = CARTESIAN_POINT ( 'NONE',  ( 0.3334645669291338987, -9.254566434645669797E-06, -2.341456692880161228 ) ) ;
#2013 = CARTESIAN_POINT ( 'NONE',  ( 0.4225434286521223548, -0.3242892624567478843, 1.747047244094488194 ) ) ;
#2014 = EDGE_CURVE ( 'NONE', #22651, #5888, #26397, .T. ) ;
#2015 = CARTESIAN_POINT ( 'NONE',  ( -0.6299212598425196763, 0.000000000000000000, -4.370956692913385731E-17 ) ) ;
#2016 = DIRECTION ( 'NONE',  ( 0.000000000000000000, 0.000000000000000000, -1.000000000000000000 ) ) ;
#2017 = EDGE_LOOP ( 'NONE', ( #1840, #6428 ) ) ;
#2018 = VECTOR ( 'NONE', #6496, 39.37007874015748143 ) ;
#2019 = DIRECTION ( 'NONE',  ( 0.000000000000000000, 0.000000000000000000, 1.000000000000000000 ) ) ;
#2020 = AXIS2_PLACEMENT_3D ( 'NONE', #5757, #7869, #12099 ) ;
#2021 = DIRECTION ( 'NONE',  ( 0.000000000000000000, 1.000000000000000000, 0.000000000000000000 ) ) ;
#2022 = CARTESIAN_POINT ( 'NONE',  ( 0.3339160553493882300, 0.7867001919223544082, -0.8344257386302499357 ) ) ;
#2023 = CARTESIAN_POINT ( 'NONE',  ( -0.6205631318075456315, -0.4724394499398413827, -0.9954595798869798617 ) ) ;
#2024 = ORIENTED_EDGE ( 'NONE', *, *, #17439, .T. ) ;
#2025 = DIRECTION ( 'NONE',  ( -0.000000000000000000, 0.000000000000000000, -1.000000000000000000 ) ) ;
#2026 = LINE ( 'NONE', #12899, #6921 ) ;
#2027 = DIRECTION ( 'NONE',  ( 1.000000000000000000, 0.000000000000000000, 0.000000000000000000 ) ) ;
#2028 = CARTESIAN_POINT ( 'NONE',  ( 0.2180862235769585322, 0.4423390553432415273, -1.550196850393700920 ) ) ;
#2029 = DIMENSIONAL_EXPONENTS ( 1.000000000000000000, 0.000000000000000000, 0.000000000000000000, 0.000000000000000000, 0.000000000000000000, 0.000000000000000000, 0.000000000000000000 ) ;
#2030 = TOROIDAL_SURFACE ( 'NONE', #19168, 0.3070866141732283561, 0.01181102362204724393 ) ;
#2031 = DIRECTION ( 'NONE',  ( 1.224646799147353207E-16, 1.000000000000000000, -0.000000000000000000 ) ) ;
#2032 = CARTESIAN_POINT ( 'NONE',  ( 0.2991932138496286586, -0.3411003281197161341, -1.934055118110236338 ) ) ;
#2033 = CARTESIAN_POINT ( 'NONE',  ( 0.3346456692913385988, 2.049113738730807321E-17, 1.973425196850393970 ) ) ;
#2034 = CARTESIAN_POINT ( 'NONE',  ( -0.1432577568504646015, 0.4218945342797250642, -1.934055118110236338 ) ) ;
#2035 = EDGE_CURVE ( 'NONE', #27384, #13133, #7268, .T. ) ;
#2036 = AXIS2_PLACEMENT_3D ( 'NONE', #3197, #18743, #11830 ) ;
#2037 = CARTESIAN_POINT ( 'NONE',  ( 0.3031496062992122820, 3.712511950171106268E-17, -0.4448818897637791814 ) ) ;
#2038 = AXIS2_PLACEMENT_3D ( 'NONE', #19503, #66, #8628 ) ;
#2039 = CARTESIAN_POINT ( 'NONE',  ( -0.5439522672647024715, -0.3991687350992441097, 0.1730343859005041562 ) ) ;
#2040 = CARTESIAN_POINT ( 'NONE',  ( 0.5280699926562971713, -0.06957181182499251604, 1.747047244094488194 ) ) ;
#2041 = CARTESIAN_POINT ( 'NONE',  ( -0.4922996667773635315, 0.08741303158497767956, 0.1496602734588148298 ) ) ;
#2042 = CARTESIAN_POINT ( 'NONE',  ( -0.1606879121748897576, -0.4409237942971110380, 0.07637549214372835182 ) ) ;
#2043 = EDGE_CURVE ( 'NONE', #17434, #11924, #21465, .T. ) ;
#2044 = DIRECTION ( 'NONE',  ( 1.000000000000000000, 0.000000000000000000, 0.000000000000000000 ) ) ;
#2045 = CARTESIAN_POINT ( 'NONE',  ( -0.3858827008516800827, 0.2227458012932893583, -1.934055118110236560 ) ) ;
#2046 = VECTOR ( 'NONE', #3128, 39.37007874015748143 ) ;
#2047 = ORIENTED_EDGE ( 'NONE', *, *, #11733, .T. ) ;
#2048 = CARTESIAN_POINT ( 'NONE',  ( 0.3184841198566246701, -0.1570220809524502659, 1.953740157480315043 ) ) ;
#2049 = VERTEX_POINT ( 'NONE', #7046 ) ;
#2050 = B_SPLINE_CURVE_WITH_KNOTS ( 'NONE', 3,
 ( #2022, #4684, #4431, #21940 ),
 .UNSPECIFIED., .F., .F.,
 ( 4, 4 ),
 ( -1.199999999999999956, 0.000000000000000000 ),
 .UNSPECIFIED. ) ;
#2051 = CARTESIAN_POINT ( 'NONE',  ( -0.5255103840667624260, -0.2955129232484599577, -0.2915374615789483315 ) ) ;
#2052 = CARTESIAN_POINT ( 'NONE',  ( -0.5572789388083557727, -0.3225230913466954896, 0.1183902030405236949 ) ) ;
#2053 = CARTESIAN_POINT ( 'NONE',  ( 0.07472527936312040042, -0.5671862884095228985, 0.9399606299212598381 ) ) ;
#2054 = DIRECTION ( 'NONE',  ( -1.000000000000000000, 0.000000000000000000, 0.000000000000000000 ) ) ;
#2055 = CARTESIAN_POINT ( 'NONE',  ( 0.1120675189988346587, -0.4694218845611126678, -0.3846748511993472452 ) ) ;
#2056 = CARTESIAN_POINT ( 'NONE',  ( -0.4456396174367268093, -1.277930342114489576E-27, -0.1696422624804970747 ) ) ;
#2057 = CARTESIAN_POINT ( 'NONE',  ( 0.3606190329934327310, 0.4297690281277732338, 0.1771653543307086520 ) ) ;
#2058 = AXIS2_PLACEMENT_3D ( 'NONE', #16152, #15733, #24751 ) ;
#2059 = CARTESIAN_POINT ( 'NONE',  ( 0.3606853515406420185, -0.09660931395005377398, -3.115157480314960647 ) ) ;
#2060 = VECTOR ( 'NONE', #15684, 39.37007874015748143 ) ;
#2061 = CARTESIAN_POINT ( 'NONE',  ( 0.000000000000000000, 0.000000000000000000, -3.278217716535432842E-17 ) ) ;
#2062 = DIRECTION ( 'NONE',  ( 1.000000000000000000, 0.000000000000000000, 0.000000000000000000 ) ) ;
#2063 = CARTESIAN_POINT ( 'NONE',  ( 0.006151574803149606648, 0.000000000000000000, 0.000000000000000000 ) ) ;
#2064 = PLANE ( 'NONE',  #7665 ) ;
#2065 = CARTESIAN_POINT ( 'NONE',  ( 0.2478439864030018147, -0.4300129863948118913, -1.569881889763779625 ) ) ;
#2066 = EDGE_CURVE ( 'NONE', #2885, #6378, #9145, .T. ) ;
#2067 = AXIS2_PLACEMENT_3D ( 'NONE', #10228, #4171, #8271 ) ;
#2068 = EDGE_LOOP ( 'NONE', ( #14115, #15701, #8761 ) ) ;
#2069 = CARTESIAN_POINT ( 'NONE',  ( 0.5118110236220473341, 6.402768735150616610E-17, -1.550196850393700920 ) ) ;
#2070 = EDGE_CURVE ( 'NONE', #17929, #16979, #5269, .T. ) ;
#2071 = ORIENTED_EDGE ( 'NONE', *, *, #12180, .F. ) ;
#2072 = ORIENTED_EDGE ( 'NONE', *, *, #18545, .F. ) ;
#2073 = EDGE_CURVE ( 'NONE', #8851, #9496, #18343, .T. ) ;
#2074 = DIRECTION ( 'NONE',  ( 1.000000000000000000, 0.000000000000000000, 0.000000000000000000 ) ) ;
#2075 = CARTESIAN_POINT ( 'NONE',  ( 0.5144970376935932288, -0.1378076643338853879, 1.747047244094488194 ) ) ;
#2076 = APPLICATION_PROTOCOL_DEFINITION ( 'draft international standard', 'automotive_design', 1998, #6560 ) ;
#2077 = CARTESIAN_POINT ( 'NONE',  ( -0.3121994997598258603, -0.4069448477556126265, 1.766732283464566899 ) ) ;
#2078 = ADVANCED_FACE ( 'NONE', ( #17888 ), #5190, .F. ) ;
#2079 = CARTESIAN_POINT ( 'NONE',  ( -0.5708661417322835607, 1.112204724409448842, -1.362057955744595713E-16 ) ) ;
#2080 = EDGE_LOOP ( 'NONE', ( #7272, #15062, #27209, #14683, #12115, #6957 ) ) ;
#2081 = EDGE_LOOP ( 'NONE', ( #12866, #14072, #25975, #11994 ) ) ;
#2083 = CARTESIAN_POINT ( 'NONE',  ( 0.3460635936744816399, 0.09269288654273792616, -3.115157480314960647 ) ) ;
#2082 = CARTESIAN_POINT ( 'NONE',  ( -0.6889763779527560139, 0.000000000000000000, -0.01377952755905511792 ) ) ;
#2084 = ORIENTED_EDGE ( 'NONE', *, *, #7458, .F. ) ;
#2085 = EDGE_CURVE ( 'NONE', #21339, #11020, #11517, .T. ) ;
#2086 = CIRCLE ( 'NONE', #19695, 0.5905511811023621549 ) ;
#2087 = ORIENTED_EDGE ( 'NONE', *, *, #5920, .F. ) ;
#2088 = CARTESIAN_POINT ( 'NONE',  ( -0.1599629598573265865, -0.4411872753632007926, 0.1992125984251968684 ) ) ;
#2089 = DIRECTION ( 'NONE',  ( 0.000000000000000000, 1.000000000000000000, 0.000000000000000000 ) ) ;
#2090 = CARTESIAN_POINT ( 'NONE',  ( -0.2211428102655751127, -0.2521176338356575508, 1.973425196850393970 ) ) ;
#2091 = ORIENTED_EDGE ( 'NONE', *, *, #2318, .F. ) ;
#2092 = ORIENTED_EDGE ( 'NONE', *, *, #12180, .T. ) ;
#2093 = CARTESIAN_POINT ( 'NONE',  ( -0.3707612262532960501, 0.3252100150720461658, -1.550196850393700920 ) ) ;
#2094 = DIRECTION ( 'NONE',  ( 0.000000000000000000, 0.000000000000000000, 1.000000000000000000 ) ) ;
#2095 = CARTESIAN_POINT ( 'NONE',  ( -0.5511811023622047445, 3.375010863791918375E-17, 0.9202755905511811330 ) ) ;
#2096 = ORIENTED_EDGE ( 'NONE', *, *, #13801, .T. ) ;
#2097 = ORIENTED_EDGE ( 'NONE', *, *, #16708, .F. ) ;
#2098 = ORIENTED_EDGE ( 'NONE', *, *, #19489, .F. ) ;
#2099 = CARTESIAN_POINT ( 'NONE',  ( 0.3843128886798082844, 0.1418101685956718039, -0.2362204724398992428 ) ) ;
#2100 = CARTESIAN_POINT ( 'NONE',  ( 0.4895462770359960136, 1.042587244177305195, -0.2949132003431567117 ) ) ;
#2101 = CARTESIAN_POINT ( 'NONE',  ( -0.3149606299212598381, 0.000000000000000000, 0.000000000000000000 ) ) ;
#2102 = CARTESIAN_POINT ( 'NONE',  ( 0.000000000000000000, 0.9055118110236221041, 0.000000000000000000 ) ) ;
#2103 = EDGE_LOOP ( 'NONE', ( #16313, #11756, #24, #10103 ) ) ;
#2104 = PRODUCT_DEFINITION_FORMATION_WITH_SPECIFIED_SOURCE ( 'ANY', '', #22884, .NOT_KNOWN. ) ;
#2105 = CARTESIAN_POINT ( 'NONE',  ( -0.6708784387195275700, -0.1533826961018543433, 0.1322810039474933141 ) ) ;
#2106 = CIRCLE ( 'NONE', #21510, 0.4692913385826771866 ) ;
#2107 = CARTESIAN_POINT ( 'NONE',  ( -0.5681815575442429322, 1.113574658101619930, 0.05417226358512977624 ) ) ;
#2108 = DIRECTION ( 'NONE',  ( 0.000000000000000000, 0.000000000000000000, 1.000000000000000000 ) ) ;
#2109 = ADVANCED_FACE ( 'NONE', ( #3781, #3200 ), #3629, .T. ) ;
#2110 = TOROIDAL_SURFACE ( 'NONE', #20597, 0.4232283464566928832, 0.07677165354330708902 ) ;
#2111 = B_SPLINE_CURVE_WITH_KNOTS ( 'NONE', 3,
 ( #16128, #24724, #22619, #14740, #10455, #27279 ),
 .UNSPECIFIED., .F., .F.,
 ( 4, 2, 4 ),
 ( 0.5000000000000000000, 0.7500000000000000000, 1.000000000000000000 ),
 .UNSPECIFIED. ) ;
#2112 = CARTESIAN_POINT ( 'NONE',  ( -0.3872945158171015589, 0.000000000000000000, -0.2204724409448818867 ) ) ;
#2113 = CARTESIAN_POINT ( 'NONE',  ( -0.1318897637674579792, 1.615183770381179830E-17, 0.9055118110027171596 ) ) ;
#2114 = CARTESIAN_POINT ( 'NONE',  ( -0.05118110236220472370, 0.000000000000000000, 0.000000000000000000 ) ) ;
#2115 = EDGE_CURVE ( 'NONE', #20796, #18835, #23260, .T. ) ;
#2116 = CARTESIAN_POINT ( 'NONE',  ( -0.06296589279854497567, 0.1968503937007873850, -3.224248289462050998 ) ) ;
#2117 = ORIENTED_EDGE ( 'NONE', *, *, #24084, .F. ) ;
#2118 = CARTESIAN_POINT ( 'NONE',  ( 0.3197948809237959322, -0.6622502000717108706, 0.2763636194327128148 ) ) ;
#2119 = B_SPLINE_CURVE_WITH_KNOTS ( 'NONE', 3,
 ( #16214, #7741, #12392, #13956, #22567, #20730 ),
 .UNSPECIFIED., .F., .F.,
 ( 4, 2, 4 ),
 ( 0.000000000000000000, 0.2500000000000000000, 0.5000000000000000000 ),
 .UNSPECIFIED. ) ;
#2120 = EDGE_LOOP ( 'NONE', ( #5122, #17750, #15437, #8046 ) ) ;
#2121 = AXIS2_PLACEMENT_3D ( 'NONE', #25906, #19405, #13042 ) ;
#2122 = ORIENTED_EDGE ( 'NONE', *, *, #5680, .F. ) ;
#2123 = CARTESIAN_POINT ( 'NONE',  ( 0.4931105264837953306, 0.08735026989778582607, 0.09684874903502814492 ) ) ;
#2124 = AXIS2_PLACEMENT_3D ( 'NONE', #13217, #12672, #11106 ) ;
#2125 = DIRECTION ( 'NONE',  ( -0.1736481776669299426, 0.9848077530122081313, 0.000000000000000000 ) ) ;
#2126 = CARTESIAN_POINT ( 'NONE',  ( 0.4783323773986672967, -0.2762247810518773106, 0.9202755905511811330 ) ) ;
#2127 = ORIENTED_EDGE ( 'NONE', *, *, #27252, .T. ) ;
#2128 = CARTESIAN_POINT ( 'NONE',  ( 0.000000000000000000, 0.000000000000000000, -1.092739370078740131E-17 ) ) ;
#2129 = ORIENTED_EDGE ( 'NONE', *, *, #13165, .F. ) ;
#2130 = DIRECTION ( 'NONE',  ( 0.000000000000000000, 0.000000000000000000, -1.000000000000000000 ) ) ;
#2131 = CARTESIAN_POINT ( 'NONE',  ( -0.2979095355689177493, -0.6203660015065670663, 0.1322834645669291320 ) ) ;
#2132 = CARTESIAN_POINT ( 'NONE',  ( -0.3722026523000413478, 0.000000000000000000, -0.1033464566929133965 ) ) ;
#2133 = DIRECTION ( 'NONE',  ( 1.000000000000000000, 0.000000000000000000, 0.000000000000000000 ) ) ;
#2134 = CARTESIAN_POINT ( 'NONE',  ( 0.000000000000000000, 0.6881889763779527325, 0.1322810039474933141 ) ) ;
#2135 = ORIENTED_EDGE ( 'NONE', *, *, #21289, .T. ) ;
#2136 = CARTESIAN_POINT ( 'NONE',  ( -0.09842519685039370636, 0.2165354330708661457, -3.548228346456693050 ) ) ;
#2137 = CARTESIAN_POINT ( 'NONE',  ( 0.6241887519799541595, 0.3029073140874564696, 0.5246508579836981490 ) ) ;
#2138 = DIRECTION ( 'NONE',  ( 0.000000000000000000, 0.000000000000000000, 1.000000000000000000 ) ) ;
#2139 = DIRECTION ( 'NONE',  ( -0.000000000000000000, -0.000000000000000000, -1.000000000000000000 ) ) ;
#2140 = DIRECTION ( 'NONE',  ( 0.000000000000000000, 1.000000000000000000, 0.000000000000000000 ) ) ;
#2141 = EDGE_CURVE ( 'NONE', #20556, #17614, #19275, .T. ) ;
#2142 = CARTESIAN_POINT ( 'NONE',  ( 0.3334645669291338987, -0.8041772776331653771, -0.9118913923173522784 ) ) ;
#2143 = CARTESIAN_POINT ( 'NONE',  ( 0.3482225189666513510, -0.4539000224940975547, 0.9399606299212598381 ) ) ;
#2144 = AXIS2_PLACEMENT_3D ( 'NONE', #16295, #20803, #18383 ) ;
#2145 = ( GEOMETRIC_REPRESENTATION_CONTEXT ( 3 ) GLOBAL_UNCERTAINTY_ASSIGNED_CONTEXT ( ( #24851 ) ) GLOBAL_UNIT_ASSIGNED_CONTEXT ( ( #26069, #23822, #10819 ) ) REPRESENTATION_CONTEXT ( 'NONE', 'WORKASPACE' ) ) ;
#2146 = ORIENTED_EDGE ( 'NONE', *, *, #14178, .T. ) ;
#2147 = PRODUCT ( 'MAS-227', 'MAS-227', '', ( #16036 ) ) ;
#2148 = CARTESIAN_POINT ( 'NONE',  ( -0.3213085410496429040, 0.1584824234588512737, -3.115157480314961091 ) ) ;
#2149 = EDGE_CURVE ( 'NONE', #23473, #158, #698, .T. ) ;
#2150 = EDGE_LOOP ( 'NONE', ( #2358, #2146 ) ) ;
#2151 = EDGE_LOOP ( 'NONE', ( #12416, #19888, #24371, #19139 ) ) ;
#2152 = CARTESIAN_POINT ( 'NONE',  ( 0.5085118447796558305, 0.06699507805605002531, -1.550196850393700920 ) ) ;
#2153 = DIRECTION ( 'NONE',  ( 1.000000000000000000, 0.000000000000000000, 0.000000000000000000 ) ) ;
#2154 = CARTESIAN_POINT ( 'NONE',  ( 0.3543307086614173040, 0.09842519685039370636, 0.000000000000000000 ) ) ;
#2155 = VERTEX_POINT ( 'NONE', #7889 ) ;
#2156 = DIRECTION ( 'NONE',  ( 0.000000000000000000, 0.000000000000000000, 1.000000000000000000 ) ) ;
#2157 = ORIENTED_EDGE ( 'NONE', *, *, #18019, .T. ) ;
#2158 = EDGE_CURVE ( 'NONE', #15240, #27472, #9611, .T. ) ;
#2159 = B_SPLINE_CURVE_WITH_KNOTS ( 'NONE', 3,
 ( #26441, #3, #7107, #13452, #8569, #15725 ),
 .UNSPECIFIED., .F., .F.,
 ( 4, 2, 4 ),
 ( 0.5000000000000000000, 0.7500000000000000000, 1.000000000000000000 ),
 .UNSPECIFIED. ) ;
#2160 = FACE_OUTER_BOUND ( 'NONE', #7511, .T. ) ;
#2161 = AXIS2_PLACEMENT_3D ( 'NONE', #16671, #14425, #3810 ) ;
#2162 = AXIS2_PLACEMENT_3D ( 'NONE', #917, #9504, #7127 ) ;
#2163 = CARTESIAN_POINT ( 'NONE',  ( -0.5118110236220472231, 0.000000000000000000, -0.2618110236220472231 ) ) ;
#2164 = CARTESIAN_POINT ( 'NONE',  ( 0.3334645669291338987, -1.243457723967850148, -0.6813714283177954023 ) ) ;
#2165 = ORIENTED_EDGE ( 'NONE', *, *, #5688, .F. ) ;
#2166 = SURFACE_SIDE_STYLE ('',( #25102 ) ) ;
#2167 = CARTESIAN_POINT ( 'NONE',  ( 0.000000000000000000, 0.000000000000000000, 0.2362204724409449064 ) ) ;
#2168 = AXIS2_PLACEMENT_3D ( 'NONE', #14327, #14631, #1598 ) ;
#2169 = ORIENTED_EDGE ( 'NONE', *, *, #348, .F. ) ;
#2170 = CARTESIAN_POINT ( 'NONE',  ( 0.000000000000000000, 0.07874015748662489822, 0.000000000000000000 ) ) ;
#2171 = CARTESIAN_POINT ( 'NONE',  ( 0.06894484415258525511, 0.05111597790624471116, -0.4724409448841456749 ) ) ;
#2172 = CARTESIAN_POINT ( 'NONE',  ( -0.3707612262533165337, -0.3252100150720257932, -1.569881889763779625 ) ) ;
#2173 = CARTESIAN_POINT ( 'NONE',  ( -0.4585215200179055817, 0.000000000000000000, -1.928289503579156516 ) ) ;
#2174 = CARTESIAN_POINT ( 'NONE',  ( 0.4986013261500205074, 6.106105181202481056E-17, -0.05511811023622047168 ) ) ;
#2175 = EDGE_CURVE ( 'NONE', #3772, #3172, #5916, .T. ) ;
#2176 = AXIS2_PLACEMENT_3D ( 'NONE', #25126, #20756, #23318 ) ;
#2177 = LINE ( 'NONE', #19551, #13048 ) ;
#2178 = CARTESIAN_POINT ( 'NONE',  ( -0.09842519685039370636, 0.07874015748031495954, -0.04546065111729338803 ) ) ;
#2179 = EDGE_CURVE ( 'NONE', #14125, #1064, #15162, .T. ) ;
#2180 = AXIS2_PLACEMENT_3D ( 'NONE', #21071, #20654, #10050 ) ;
#2181 = EDGE_LOOP ( 'NONE', ( #2379, #22153 ) ) ;
#2182 = VECTOR ( 'NONE', #21944, 39.37007874015748143 ) ;
#2183 = CARTESIAN_POINT ( 'NONE',  ( -0.5632721120450597807, -0.3296178001376885436, 0.1935414926636310762 ) ) ;
#2184 = FACE_BOUND ( 'NONE', #13764, .T. ) ;
#2185 = CARTESIAN_POINT ( 'NONE',  ( -0.09842519685039370636, 0.2165354330708661457, -3.548228346456693050 ) ) ;
#2186 = LINE ( 'NONE', #14929, #19182 ) ;
#2187 = CARTESIAN_POINT ( 'NONE',  ( 0.3995913070738940642, 0.1970988029425181920, -1.934055118110236338 ) ) ;
#2188 = ORIENTED_EDGE ( 'NONE', *, *, #7551, .T. ) ;
#2189 = CARTESIAN_POINT ( 'NONE',  ( -0.7432982829791772161, 0.2816507422265389637, 0.04372923255535362402 ) ) ;
#2190 = VERTEX_POINT ( 'NONE', #21015 ) ;
#2191 = CARTESIAN_POINT ( 'NONE',  ( 0.000000000000000000, 0.000000000000000000, -0.2618110236220472231 ) ) ;
#2192 = CARTESIAN_POINT ( 'NONE',  ( 0.5190862322091315262, -0.1177929122753177127, 0.1322834645669291320 ) ) ;
#2193 = B_SPLINE_CURVE_WITH_KNOTS ( 'NONE', 3,
 ( #1042, #15735, #20099, #14032, #26319, #20526, #15859, #17831, #13599, #5265 ),
 .UNSPECIFIED., .F., .F.,
 ( 4, 2, 2, 2, 4 ),
 ( 0.000000000000000000, 0.2500000000000000000, 0.5000000000000000000, 0.7500000000000000000, 1.000000000000000000 ),
 .UNSPECIFIED. ) ;
#2194 = LINE ( 'NONE', #8827, #18525 ) ;
#2195 = EDGE_CURVE ( 'NONE', #19740, #12947, #25112, .T. ) ;
#2196 = DIRECTION ( 'NONE',  ( 1.000000000000000000, 0.000000000000000000, 0.000000000000000000 ) ) ;
#2197 = CARTESIAN_POINT ( 'NONE',  ( 0.3606853515406215904, 0.09660931395005435685, -3.115157480314960647 ) ) ;
#2198 = LINE ( 'NONE', #2975, #8961 ) ;
#2199 = AXIS2_PLACEMENT_3D ( 'NONE', #24532, #20307, #18304 ) ;
#2200 = SURFACE_STYLE_FILL_AREA ( #4325 ) ;
#2201 = FACE_BOUND ( 'NONE', #13567, .T. ) ;
#2202 = DIRECTION ( 'NONE',  ( 0.000000000000000000, -1.000000000000000000, 0.000000000000000000 ) ) ;
#2203 = AXIS2_PLACEMENT_3D ( 'NONE', #11919, #13750, #9357 ) ;
#2204 = VERTEX_POINT ( 'NONE', #22715 ) ;
#2205 = EDGE_LOOP ( 'NONE', ( #5369, #6270, #18830, #662 ) ) ;
#2206 = CARTESIAN_POINT ( 'NONE',  ( -0.6299212598425196763, -0.6348133144914134274, -0.8891632684400255782 ) ) ;
#2207 = CARTESIAN_POINT ( 'NONE',  ( 0.4092783051644228731, 0.3145317858139328182, 1.766732283464566899 ) ) ;
#2208 = CARTESIAN_POINT ( 'NONE',  ( 0.3680051700917442714, -0.2263466406172265633, -0.3920438816715692831 ) ) ;
#2209 = CARTESIAN_POINT ( 'NONE',  ( -0.3382184156732166436, 0.3855916753051391033, 1.766732283464566899 ) ) ;
#2210 = DIRECTION ( 'NONE',  ( 7.017815000000000124E-18, -1.000000000000000000, 0.000000000000000000 ) ) ;
#2211 = CIRCLE ( 'NONE', #10787, 0.2952755905264887182 ) ;
#2212 = EDGE_LOOP ( 'NONE', ( #12586, #23625, #17128, #15554 ) ) ;
#2213 = VERTEX_POINT ( 'NONE', #10133 ) ;
#2214 = CARTESIAN_POINT ( 'NONE',  ( -0.04679574315772456333, -0.3551931031211519874, -3.115157480314960647 ) ) ;
#2215 = ORIENTED_EDGE ( 'NONE', *, *, #25261, .F. ) ;
#2217 = AXIS2_PLACEMENT_3D ( 'NONE', #27293, #25163, #7943 ) ;
#2218 = ORIENTED_EDGE ( 'NONE', *, *, #241, .T. ) ;
#2219 = CARTESIAN_POINT ( 'NONE',  ( 0.5869493968219645641, -0.2133897621573078718, -0.3696019098714952711 ) ) ;
#2220 = ( LENGTH_UNIT ( ) NAMED_UNIT ( * ) SI_UNIT ( $, .METRE. ) ) ;
#2221 = CARTESIAN_POINT ( 'NONE',  ( 0.3339160553493882300, 0.9384519710407874804, -0.7923371756411300426 ) ) ;
#2222 = VERTEX_POINT ( 'NONE', #5776 ) ;
#2223 = VERTEX_POINT ( 'NONE', #14401 ) ;
#2224 = DIRECTION ( 'NONE',  ( -1.000000000000000000, 0.000000000000000000, 0.000000000000000000 ) ) ;
#2225 = VERTEX_POINT ( 'NONE', #20456 ) ;
#2226 = B_SPLINE_CURVE_WITH_KNOTS ( 'NONE', 3,
 ( #2337, #9236, #20129, #19859, #23963, #7142 ),
 .UNSPECIFIED., .F., .F.,
 ( 4, 2, 4 ),
 ( 0.3864984308775630262, 0.3881911340211379735, 0.3898838371647110335 ),
 .UNSPECIFIED. ) ;
#2227 = ORIENTED_EDGE ( 'NONE', *, *, #22042, .F. ) ;
#2228 = ORIENTED_EDGE ( 'NONE', *, *, #17985, .F. ) ;
#2229 = EDGE_CURVE ( 'NONE', #17886, #21686, #2935, .T. ) ;
#2230 = CARTESIAN_POINT ( 'NONE',  ( 0.3020979083622633565, 0.3591256245826334181, 0.07637795275590551769 ) ) ;
#2231 = CARTESIAN_POINT ( 'NONE',  ( 0.3751294191746885609, 0.2999672986753447734, 0.2362204724409446843 ) ) ;
#2232 = CARTESIAN_POINT ( 'NONE',  ( 0.3992017438595159562, -0.2298214351608004746, 0.1771653543307084855 ) ) ;
#2233 = EDGE_CURVE ( 'NONE', #20284, #17070, #24466, .T. ) ;
#2234 = CIRCLE ( 'NONE', #23000, 0.5007874015748031704 ) ;
#2235 = DIRECTION ( 'NONE',  ( 1.000000000000000000, 0.000000000000000000, 0.000000000000000000 ) ) ;
#2236 = ADVANCED_FACE ( 'NONE', ( #27103 ), #25129, .T. ) ;
#2237 = VECTOR ( 'NONE', #11282, 39.37007874015748143 ) ;
#2238 = DIRECTION ( 'NONE',  ( 0.000000000000000000, 7.180547322999998243E-06, 0.9999999999742198442 ) ) ;
#2239 = CARTESIAN_POINT ( 'NONE',  ( -0.06002032661671147240, 0.4585215200179056372, -1.928289503579156516 ) ) ;
#2240 = CARTESIAN_POINT ( 'NONE',  ( -0.5996943638624113726, 0.000000000000000000, -0.2480314960629921295 ) ) ;
#2241 = CARTESIAN_POINT ( 'NONE',  ( -0.6003937007829848183, 1.122047244090071727, 1.315345636034250449E-15 ) ) ;
#2242 = DIRECTION ( 'NONE',  ( 0.000000000000000000, 0.000000000000000000, 1.000000000000000000 ) ) ;
#2243 = CARTESIAN_POINT ( 'NONE',  ( -0.06048688226689048764, 0.1968503937007873850, -3.193930429277412220 ) ) ;
#2244 = ORIENTED_EDGE ( 'NONE', *, *, #3504, .T. ) ;
#2245 = CARTESIAN_POINT ( 'NONE',  ( 0.4021324607160879361, 0.3215300179764621347, 0.1473214333187666258 ) ) ;
#2246 = AXIS2_PLACEMENT_3D ( 'NONE', #2393, #11022, #319 ) ;
#2247 = VERTEX_POINT ( 'NONE', #1349 ) ;
#2248 = ORIENTED_EDGE ( 'NONE', *, *, #17807, .F. ) ;
#2249 = B_SPLINE_CURVE_WITH_KNOTS ( 'NONE', 3,
 ( #9499, #22373, #2857, #13896, #18094, #2996, #27040, #11628, #7394, #12055 ),
 .UNSPECIFIED., .F., .F.,
 ( 4, 2, 2, 2, 4 ),
 ( 0.000000000000000000, 0.2500000000000001665, 0.5000000000000003331, 0.7500000000000001110, 1.000000000000000000 ),
 .UNSPECIFIED. ) ;
#2250 = AXIS2_PLACEMENT_3D ( 'NONE', #1266, #16241, #9871 ) ;
#2251 = CARTESIAN_POINT ( 'NONE',  ( 0.4446020952038907681, 5.549066237130534971E-17, -1.934055118110236338 ) ) ;
#2252 = FACE_OUTER_BOUND ( 'NONE', #17, .T. ) ;
#2253 = DIRECTION ( 'NONE',  ( 1.000000000000000000, 0.000000000000000000, 0.000000000000000000 ) ) ;
#2254 = ORIENTED_EDGE ( 'NONE', *, *, #24577, .T. ) ;
#2255 = CARTESIAN_POINT ( 'NONE',  ( 0.4382482975805169212, -0.3362148458988646338, 0.9202755905511811330 ) ) ;
#2256 = CARTESIAN_POINT ( 'NONE',  ( 0.6241887519799541595, -0.6058146281749130502, 6.299353404003403643E-17 ) ) ;
#2257 = ORIENTED_EDGE ( 'NONE', *, *, #23536, .F. ) ;
#2258 = ADVANCED_FACE ( 'NONE', ( #7995 ), #16600, .F. ) ;
#2259 = CARTESIAN_POINT ( 'NONE',  ( 0.000000000000000000, 0.000000000000000000, -0.4724409448818898127 ) ) ;
#2260 = CARTESIAN_POINT ( 'NONE',  ( 0.2256712916308122319, 0.000000000000000000, -4.330708661396418080 ) ) ;
#2261 = DIRECTION ( 'NONE',  ( 0.000000000000000000, 0.000000000000000000, 1.000000000000000000 ) ) ;
#2262 = CARTESIAN_POINT ( 'NONE',  ( 0.000000000000000000, 0.000000000000000000, -0.1309055118110236116 ) ) ;
#2263 = CARTESIAN_POINT ( 'NONE',  ( 0.3334645669291338987, -5.862181872598426086E-06, -1.869015748010449007 ) ) ;
#2264 = ADVANCED_FACE ( 'NONE', ( #19133 ), #3370, .T. ) ;
#2265 = CARTESIAN_POINT ( 'NONE',  ( 0.000000000000000000, 0.6881889763779527325, -1.092739370078740131E-17 ) ) ;
#2266 = CARTESIAN_POINT ( 'NONE',  ( -0.09842519685039370636, 0.2165354330708661457, -3.364501312335955063 ) ) ;
#2267 = CARTESIAN_POINT ( 'NONE',  ( 0.000000000000000000, 0.000000000000000000, -0.07578740157480315376 ) ) ;
#2268 = EDGE_CURVE ( 'NONE', #11692, #16657, #22347, .T. ) ;
#2269 = CARTESIAN_POINT ( 'NONE',  ( 0.000000000000000000, 0.000000000000000000, 0.2574803149606298969 ) ) ;
#2270 = CARTESIAN_POINT ( 'NONE',  ( 0.03937007874015747977, 0.000000000000000000, 0.000000000000000000 ) ) ;
#2271 = FACE_BOUND ( 'NONE', #4134, .T. ) ;
#2272 = CARTESIAN_POINT ( 'NONE',  ( -0.09842519685039370636, -0.07874015748031495954, -0.04546065111729338803 ) ) ;
#2273 = AXIS2_PLACEMENT_3D ( 'NONE', #26937, #2903, #20015 ) ;
#2274 = CARTESIAN_POINT ( 'NONE',  ( -0.3772436174784328244, 0.4300830224589641260, 0.9399606299212598381 ) ) ;
#2275 = DIRECTION ( 'NONE',  ( 0.000000000000000000, 0.000000000000000000, 1.000000000000000000 ) ) ;
#2276 = ORIENTED_EDGE ( 'NONE', *, *, #7179, .T. ) ;
#2277 = CARTESIAN_POINT ( 'NONE',  ( -0.1610509776512037416, -0.4407912692718771175, 0.07637795275590551769 ) ) ;
#2278 = EDGE_CURVE ( 'NONE', #15470, #23305, #13037, .T. ) ;
#2279 = STYLED_ITEM ( 'NONE', ( #12321 ), #12108 ) ;
#2280 = ORIENTED_EDGE ( 'NONE', *, *, #17574, .F. ) ;
#2281 = VERTEX_POINT ( 'NONE', #23539 ) ;
#2282 = CARTESIAN_POINT ( 'NONE',  ( -0.3912931228432058872, -0.3001918266902326993, -1.550196850393700920 ) ) ;
#2283 = CARTESIAN_POINT ( 'NONE',  ( -0.4538422614037148084, -0.3483115186076898295, 0.9399606299212598381 ) ) ;
#2284 = DIRECTION ( 'NONE',  ( 0.000000000000000000, 0.000000000000000000, -1.000000000000000000 ) ) ;
#2285 = ORIENTED_EDGE ( 'NONE', *, *, #21450, .F. ) ;
#2286 = CARTESIAN_POINT ( 'NONE',  ( 0.000000000000000000, 0.2952755905511810774, 0.01181102362204724393 ) ) ;
#2287 = ADVANCED_FACE ( 'NONE', ( #12776 ), #25780, .T. ) ;
#2288 = B_SPLINE_CURVE_WITH_KNOTS ( 'NONE', 3,
 ( #13606, #26190, #6848, #13061, #6989, #248 ),
 .UNSPECIFIED., .F., .F.,
 ( 4, 2, 4 ),
 ( 0.9359046326922999537, 0.9375808709372039917, 0.9392571091821070306 ),
 .UNSPECIFIED. ) ;
#2289 = FILL_AREA_STYLE_COLOUR ( '', #8101 ) ;
#2290 = AXIS2_PLACEMENT_3D ( 'NONE', #20850, #5604, #16474 ) ;
#2291 = CARTESIAN_POINT ( 'NONE',  ( 0.3905379133858267737, 0.2805118110236220486, -0.4858607088160732390 ) ) ;
#2292 = CARTESIAN_POINT ( 'NONE',  ( 0.4133615125893445597, 0.4936731914951132949, 0.1183902030404491851 ) ) ;
#2293 = EDGE_CURVE ( 'NONE', #20801, #20760, #12897, .T. ) ;
#2294 = CARTESIAN_POINT ( 'NONE',  ( 0.003937007874015826907, 7.887824528841537495E-18, 0.09842519685039370636 ) ) ;
#2295 = CARTESIAN_POINT ( 'NONE',  ( 0.2979095355690402069, -0.6203660015065080024, 0.1322834645669291320 ) ) ;
#2296 = CARTESIAN_POINT ( 'NONE',  ( -9.069736220472442904E-16, -0.8267716535433071723, 0.000000000000000000 ) ) ;
#2297 = CARTESIAN_POINT ( 'NONE',  ( 0.06441834428466734763, 0.4889536969035060965, -1.550196850393700920 ) ) ;
#2298 = EDGE_CURVE ( 'NONE', #19599, #5829, #18049, .T. ) ;
#2299 = CARTESIAN_POINT ( 'NONE',  ( 0.3454440660767517657, -0.3030032861724969440, -1.928289503579156516 ) ) ;
#2300 = CARTESIAN_POINT ( 'NONE',  ( 0.4438564651657277427, 0.1188866373884867045, -1.928289503579172726 ) ) ;
#2301 = DIRECTION ( 'NONE',  ( 0.000000000000000000, 0.000000000000000000, 1.000000000000000000 ) ) ;
#2302 = ADVANCED_FACE ( 'NONE', ( #27767, #15193 ), #1624, .T. ) ;
#2303 = CARTESIAN_POINT ( 'NONE',  ( -0.5744851493209846005, 0.4591414886187322741, 0.2763636194302094284 ) ) ;
#2304 = AXIS2_PLACEMENT_3D ( 'NONE', #2730, #11361, #7124 ) ;
#2305 = DIRECTION ( 'NONE',  ( -1.000000000000000000, 0.000000000000000000, 0.000000000000000000 ) ) ;
#2306 = LINE ( 'NONE', #17693, #23561 ) ;
#2307 = CARTESIAN_POINT ( 'NONE',  ( 0.4225965726693019509, -0.3242071728275352505, 1.747047244094488194 ) ) ;
#2308 = B_SPLINE_CURVE_WITH_KNOTS ( 'NONE', 3,
 ( #2134, #4396, #25868, #14201 ),
 .UNSPECIFIED., .F., .F.,
 ( 4, 4 ),
 ( 0.4064350009536160102, 0.4083596218470010308 ),
 .UNSPECIFIED. ) ;
#2309 = ORIENTED_EDGE ( 'NONE', *, *, #20542, .F. ) ;
#2310 = AXIS2_PLACEMENT_3D ( 'NONE', #7416, #9240, #16044 ) ;
#2311 = CARTESIAN_POINT ( 'NONE',  ( -0.0006615832605804723319, 0.6212594902576319411, 0.2574803149606298969 ) ) ;
#2312 = CARTESIAN_POINT ( 'NONE',  ( -0.2979095355689177493, -0.6203660015065670663, 0.3401574803149606252 ) ) ;
#2313 = ORIENTED_EDGE ( 'NONE', *, *, #26134, .F. ) ;
#2314 = FACE_OUTER_BOUND ( 'NONE', #19001, .T. ) ;
#2315 = ORIENTED_EDGE ( 'NONE', *, *, #8864, .F. ) ;
#2316 = CARTESIAN_POINT ( 'NONE',  ( -0.6996199877990079141, 0.1202923534080998086, -0.08607181623015019989 ) ) ;
#2317 = VERTEX_POINT ( 'NONE', #19276 ) ;
#2318 = EDGE_CURVE ( 'NONE', #17614, #17378, #8133, .T. ) ;
#2319 = CYLINDRICAL_SURFACE ( 'NONE', #1301, 0.1308464566929133932 ) ;
#2320 = FACE_OUTER_BOUND ( 'NONE', #11386, .T. ) ;
#2321 = CARTESIAN_POINT ( 'NONE',  ( 0.3482225189666513510, -0.4539000224940975547, 0.9399606299212598381 ) ) ;
#2322 = CARTESIAN_POINT ( 'NONE',  ( -0.4724409448465559103, 0.000000000000000000, 1.953740157480315043 ) ) ;
#2323 = EDGE_CURVE ( 'NONE', #339, #1560, #6148, .T. ) ;
#2324 = EDGE_CURVE ( 'NONE', #1867, #20809, #4761, .T. ) ;
#2325 = VECTOR ( 'NONE', #23756, 39.37007874015748143 ) ;
#2326 = CARTESIAN_POINT ( 'NONE',  ( -0.3350145293472930885, -0.2937497900410970253, -1.934055118110236338 ) ) ;
#2327 = CARTESIAN_POINT ( 'NONE',  ( -0.2807137536170348779, -0.2462256503456018430, -3.115157480314960647 ) ) ;
#2328 = ( LENGTH_UNIT ( ) NAMED_UNIT ( * ) SI_UNIT ( $, .METRE. ) ) ;
#2329 = DIRECTION ( 'NONE',  ( -0.9575713609010866323, 0.2881962678142118706, 0.000000000000000000 ) ) ;
#2330 = CARTESIAN_POINT ( 'NONE',  ( 0.000000000000000000, 0.000000000000000000, 0.1771653543307086520 ) ) ;
#2331 = EDGE_LOOP ( 'NONE', ( #5331, #5512, #8568, #18130 ) ) ;
#2332 = CYLINDRICAL_SURFACE ( 'NONE', #25371, 0.1181102362204718703 ) ;
#2333 = COLOUR_RGB ( '', 0.72549020, 0.75294118, 0.79215686) ;
#2334 = DIRECTION ( 'NONE',  ( -0.000000000000000000, -1.000000000000000000, -0.000000000000000000 ) ) ;
#2335 = ORIENTED_EDGE ( 'NONE', *, *, #25585, .F. ) ;
#2336 = ORIENTED_EDGE ( 'NONE', *, *, #12419, .F. ) ;
#2337 = CARTESIAN_POINT ( 'NONE',  ( -0.4165721057576322606, 0.3313508221749649763, 0.1322834645669291320 ) ) ;
#2338 = DIRECTION ( 'NONE',  ( -0.000000000000000000, -0.000000000000000000, -1.000000000000000000 ) ) ;
#2339 = CARTESIAN_POINT ( 'NONE',  ( 0.4600326175560556230, 0.2268096725222457644, 1.766732283464566899 ) ) ;
#2340 = CARTESIAN_POINT ( 'NONE',  ( -0.5085118447801415531, -0.06699507805368200286, 1.747047244094488194 ) ) ;
#2341 = CYLINDRICAL_SURFACE ( 'NONE', #16764, 0.1308464566929133932 ) ;
#2342 = AXIS2_PLACEMENT_3D ( 'NONE', #27069, #11801, #14070 ) ;
#2343 = ORIENTED_EDGE ( 'NONE', *, *, #14128, .T. ) ;
#2344 = AXIS2_PLACEMENT_3D ( 'NONE', #4791, #990, #13410 ) ;
#2345 = ORIENTED_EDGE ( 'NONE', *, *, #4798, .T. ) ;
#2346 = CARTESIAN_POINT ( 'NONE',  ( -0.3606853515406169275, 0.09660931395005029065, -3.115157480314960647 ) ) ;
#2347 = ORIENTED_EDGE ( 'NONE', *, *, #4905, .T. ) ;
#2348 = ORIENTED_EDGE ( 'NONE', *, *, #24166, .F. ) ;
#2349 = DIRECTION ( 'NONE',  ( 0.8660254037844390407, -0.4999999999999994449, 0.000000000000000000 ) ) ;
#2350 = DIRECTION ( 'NONE',  ( 0.000000000000000000, 1.000000000000000000, 0.000000000000000000 ) ) ;
#2351 = CARTESIAN_POINT ( 'NONE',  ( 0.3175540113612289050, 0.1078280746903826914, 1.953740157480315043 ) ) ;
#2352 = ORIENTED_EDGE ( 'NONE', *, *, #6736, .F. ) ;
#2353 = ORIENTED_EDGE ( 'NONE', *, *, #25470, .F. ) ;
#2354 = CARTESIAN_POINT ( 'NONE',  ( 0.3264619303874873313, -0.1888818218344748001, 0.1992142436757342316 ) ) ;
#2355 = FACE_OUTER_BOUND ( 'NONE', #2723, .T. ) ;
#2356 = EDGE_LOOP ( 'NONE', ( #13538, #26483, #11394, #8210 ) ) ;
#2357 = EDGE_LOOP ( 'NONE', ( #8662, #5777 ) ) ;
#2358 = ORIENTED_EDGE ( 'NONE', *, *, #12014, .F. ) ;
#2359 = CYLINDRICAL_SURFACE ( 'NONE', #4544, 0.1673228346456692994 ) ;
#2360 = EDGE_CURVE ( 'NONE', #24921, #21448, #25528, .T. ) ;
#2361 = CARTESIAN_POINT ( 'NONE',  ( -0.2228126397720058549, -0.3858397471888898589, -1.934055118110236338 ) ) ;
#2362 = FACE_OUTER_BOUND ( 'NONE', #12318, .T. ) ;
#2363 = CARTESIAN_POINT ( 'NONE',  ( -0.1968503937007874127, -0.4724409448818898127, 0.8182917201112815953 ) ) ;
#2364 = EDGE_LOOP ( 'NONE', ( #4572, #27619 ) ) ;
#2365 = CARTESIAN_POINT ( 'NONE',  ( 0.7107691196319370075, 0.7407165212924035069, 0.002142197690853237663 ) ) ;
#2366 = ORIENTED_EDGE ( 'NONE', *, *, #8607, .T. ) ;
#2367 = CIRCLE ( 'NONE', #19974, 0.6299212598425196763 ) ;
#2368 = CARTESIAN_POINT ( 'NONE',  ( -0.0006443779181928191001, 0.4960456921223007076, 0.2989974301413287905 ) ) ;
#2369 = VECTOR ( 'NONE', #13146, 39.37007874015748143 ) ;
#2370 = CARTESIAN_POINT ( 'NONE',  ( 0.000000000000000000, 0.000000000000000000, 0.5532930914870253236 ) ) ;
#2371 = DIRECTION ( 'NONE',  ( 0.000000000000000000, 0.000000000000000000, -1.000000000000000000 ) ) ;
#2372 = EDGE_CURVE ( 'NONE', #7271, #14162, #6429, .T. ) ;
#2373 = DIRECTION ( 'NONE',  ( 1.000000000000000000, 0.000000000000000000, 0.000000000000000000 ) ) ;
#2374 = EDGE_CURVE ( 'NONE', #14762, #24304, #24142, .T. ) ;
#2375 = EDGE_LOOP ( 'NONE', ( #25682, #7320, #24025, #12399, #13275, #4753 ) ) ;
#2376 = CARTESIAN_POINT ( 'NONE',  ( -0.09586345222253926657, 0.2165354330708661457, -3.246875207736367841 ) ) ;
#2377 = ORIENTED_EDGE ( 'NONE', *, *, #27274, .F. ) ;
#2378 = PRODUCT_DEFINITION ( 'UNKNOWN', '', #3426, #24918 ) ;
#2379 = ORIENTED_EDGE ( 'NONE', *, *, #15595, .T. ) ;
#2380 = CARTESIAN_POINT ( 'NONE',  ( -2.185478346456693112E-16, 0.000000000000000000, 0.000000000000000000 ) ) ;
#2381 = ADVANCED_FACE ( 'NONE', ( #111 ), #4035, .F. ) ;
#2382 = VECTOR ( 'NONE', #13266, 39.37007874015748143 ) ;
#2383 = EDGE_LOOP ( 'NONE', ( #2870, #1150, #13104, #24041 ) ) ;
#2384 = CARTESIAN_POINT ( 'NONE',  ( -0.4716107359537566324, 0.08256389912709830026, 0.08349695147708714738 ) ) ;
#2385 = VECTOR ( 'NONE', #25591, 39.37007874015748854 ) ;
#2386 = DIRECTION ( 'NONE',  ( -0.4338837391175582869, -0.9009688679024190350, 0.000000000000000000 ) ) ;
#2387 = DIRECTION ( 'NONE',  ( 0.8660254037844382635, 0.5000000000000005551, 0.000000000000000000 ) ) ;
#2388 = EDGE_CURVE ( 'NONE', #23587, #2742, #1237, .T. ) ;
#2389 = EDGE_CURVE ( 'NONE', #15780, #16922, #8394, .T. ) ;
#2390 = LINE ( 'NONE', #12852, #11209 ) ;
#2391 = ORIENTED_EDGE ( 'NONE', *, *, #8273, .T. ) ;
#2392 = CARTESIAN_POINT ( 'NONE',  ( -0.4954197419817281123, 0.2442565704126535286, 0.9399606299212598381 ) ) ;
#2393 = CARTESIAN_POINT ( 'NONE',  ( 0.000000000000000000, 0.000000000000000000, 0.9399606299212598381 ) ) ;
#2394 = VERTEX_POINT ( 'NONE', #11079 ) ;
#2395 = VECTOR ( 'NONE', #3087, 39.37007874015748854 ) ;
#2396 = CARTESIAN_POINT ( 'NONE',  ( 0.000000000000000000, 0.000000000000000000, 0.1771653543307086520 ) ) ;
#2397 = CARTESIAN_POINT ( 'NONE',  ( 0.2973550541884159570, 0.3552623538120610602, 0.2048502514842716338 ) ) ;
#2398 = CARTESIAN_POINT ( 'NONE',  ( -0.5177165354330708347, -0.4724409448818898127, 0.6411263657805708061 ) ) ;
#2399 = CARTESIAN_POINT ( 'NONE',  ( -0.2428345617565149384, 0.2885915454824177218, 0.1992125984251968684 ) ) ;
#2400 = CARTESIAN_POINT ( 'NONE',  ( 0.6708784387195275700, -0.1533826961018547319, 0.1322810039474933141 ) ) ;
#2401 = DIRECTION ( 'NONE',  ( 0.000000000000000000, 0.000000000000000000, 1.000000000000000000 ) ) ;
#2402 = CARTESIAN_POINT ( 'NONE',  ( -0.2362204724225640262, 2.892866454453686688E-17, -3.149606299191693548 ) ) ;
#2403 = CARTESIAN_POINT ( 'NONE',  ( -0.0005939837304750000086, 0.5007870493127504208, 0.09685039370078740717 ) ) ;
#2404 = CARTESIAN_POINT ( 'NONE',  ( 0.1755067523729419432, -0.3028750839302637998, -0.5245950337139047015 ) ) ;
#2405 = CARTESIAN_POINT ( 'NONE',  ( 0.000000000000000000, 0.000000000000000000, -0.2204724409448818867 ) ) ;
#2406 = CIRCLE ( 'NONE', #5580, 0.1003956692913385851 ) ;
#2407 = EDGE_LOOP ( 'NONE', ( #13278, #3298, #13573, #24116, #10984, #25647 ) ) ;
#2408 = CARTESIAN_POINT ( 'NONE',  ( 0.0001924259990422818461, 0.4692913385826771866, 0.07637549214372835182 ) ) ;
#2409 = AXIS2_PLACEMENT_3D ( 'NONE', #403, #13231, #17610 ) ;
#2410 = DIRECTION ( 'NONE',  ( 1.000000000000000000, 0.000000000000000000, 0.000000000000000000 ) ) ;
#2411 = DIRECTION ( 'NONE',  ( 1.000000000000000000, 0.000000000000000000, 0.000000000000000000 ) ) ;
#2412 = CARTESIAN_POINT ( 'NONE',  ( -0.5511811023622047445, -0.6889763779527560139, 8.437527159479796553E-17 ) ) ;
#2413 = AXIS2_PLACEMENT_3D ( 'NONE', #22706, #7306, #5180 ) ;
#2414 = LINE ( 'NONE', #2006, #23718 ) ;
#2415 = ADVANCED_FACE ( 'NONE', ( #26187 ), #7944, .T. ) ;
#2416 = VECTOR ( 'NONE', #22375, 39.37007874015748854 ) ;
#2417 = ORIENTED_EDGE ( 'NONE', *, *, #4375, .T. ) ;
#2418 = ( REPRESENTATION_RELATIONSHIP ('NONE','NONE', #12434, #20013 ) REPRESENTATION_RELATIONSHIP_WITH_TRANSFORMATION ( #25840 )SHAPE_REPRESENTATION_RELATIONSHIP( ) ) ;
#2419 = EDGE_CURVE ( 'NONE', #290, #27249, #26173, .T. ) ;
#2420 = EDGE_LOOP ( 'NONE', ( #19438, #3974, #22960, #23219, #17211, #4913 ) ) ;
#2421 = DIRECTION ( 'NONE',  ( 0.000000000000000000, 0.000000000000000000, 1.000000000000000000 ) ) ;
#2422 = EDGE_CURVE ( 'NONE', #3726, #27011, #7034, .T. ) ;
#2423 = DIRECTION ( 'NONE',  ( 1.000000000000000000, 0.000000000000000000, 0.000000000000000000 ) ) ;
#2424 = ORIENTED_EDGE ( 'NONE', *, *, #27873, .T. ) ;
#2425 = AXIS2_PLACEMENT_3D ( 'NONE', #1866, #4132, #17396 ) ;
#2426 = CARTESIAN_POINT ( 'NONE',  ( -0.2952755905511810774, 3.688404729715453115E-17, 0.01181102362204724393 ) ) ;
#2427 = EDGE_LOOP ( 'NONE', ( #10019, #27204, #13449, #9599 ) ) ;
#2428 = EDGE_LOOP ( 'NONE', ( #26101, #7798 ) ) ;
#2429 = DIRECTION ( 'NONE',  ( -1.000000000000000000, 0.000000000000000000, 0.000000000000000000 ) ) ;
#2430 = DIRECTION ( 'NONE',  ( 1.000000000000000000, 0.000000000000000000, 0.000000000000000000 ) ) ;
#2431 = FACE_OUTER_BOUND ( 'NONE', #12256, .T. ) ;
#2432 = EDGE_CURVE ( 'NONE', #12340, #4895, #14270, .T. ) ;
#2433 = DIRECTION ( 'NONE',  ( -1.000000000000000000, 0.000000000000000000, 0.000000000000000000 ) ) ;
#2434 = VECTOR ( 'NONE', #8777, 39.37007874015748143 ) ;
#2435 = CARTESIAN_POINT ( 'NONE',  ( 0.000000000000000000, 0.5511811023622047445, 0.01181102362204724393 ) ) ;
#2436 = AXIS2_PLACEMENT_3D ( 'NONE', #217, #23645, #21376 ) ;
#2437 = VERTEX_POINT ( 'NONE', #9082 ) ;
#2438 = CARTESIAN_POINT ( 'NONE',  ( -0.5708661417322835607, -0.6942509683549429322, 0.000000000000000000 ) ) ;
#2439 = CARTESIAN_POINT ( 'NONE',  ( -0.4061284506583976994, -0.2351468520617070734, 0.1992125984251968684 ) ) ;
#2440 = CARTESIAN_POINT ( 'NONE',  ( -0.2466292688015002954, -0.4270824798167766612, -1.569881889763779625 ) ) ;
#2441 = CARTESIAN_POINT ( 'NONE',  ( 0.4121342552748372690, -0.2031943647053953139, -1.928289503579153630 ) ) ;
#2442 = CARTESIAN_POINT ( 'NONE',  ( 0.000000000000000000, 0.000000000000000000, -3.278217716535432842E-17 ) ) ;
#2443 = AXIS2_PLACEMENT_3D ( 'NONE', #10155, #3225, #20485 ) ;
#2444 = CARTESIAN_POINT ( 'NONE',  ( -0.0006345105826668660581, 0.4803145415259079121, 0.2362204724409446843 ) ) ;
#2445 = ADVANCED_FACE ( 'NONE', ( #243 ), #17833, .F. ) ;
#2446 = CARTESIAN_POINT ( 'NONE',  ( -0.1918813796216842782, -0.5271897577243779276, 0.07676968503937006694 ) ) ;
#2447 = FILL_AREA_STYLE ('',( #105 ) ) ;
#2448 = CARTESIAN_POINT ( 'NONE',  ( -0.1712563538833084820, -0.5043504886477717664, 1.747047244094488194 ) ) ;
#2449 = EDGE_CURVE ( 'NONE', #14962, #17328, #26863, .T. ) ;
#2450 = CARTESIAN_POINT ( 'NONE',  ( -0.4714076450717002986, 0.08371568475170254597, 0.1920935997043449750 ) ) ;
#2451 = ORIENTED_EDGE ( 'NONE', *, *, #17265, .T. ) ;
#2452 = AXIS2_PLACEMENT_3D ( 'NONE', #16676, #18775, #6357 ) ;
#2453 = DIRECTION ( 'NONE',  ( 0.000000000000000000, 0.000000000000000000, 1.000000000000000000 ) ) ;
#2454 = TOROIDAL_SURFACE ( 'NONE', #4688, 0.4055118110236220486, 0.01181102362204724393 ) ;
#2455 = DIRECTION ( 'NONE',  ( 0.000000000000000000, 1.000000000000000000, 0.000000000000000000 ) ) ;
#2456 = EDGE_LOOP ( 'NONE', ( #3138, #14628, #3299, #24249, #2555 ) ) ;
#2457 = ORIENTED_EDGE ( 'NONE', *, *, #2066, .T. ) ;
#2458 = CARTESIAN_POINT ( 'NONE',  ( -0.6912180915490531152, 0.09686421027289587871, -0.08344423162361633284 ) ) ;
#2459 = ORIENTED_EDGE ( 'NONE', *, *, #8343, .F. ) ;
#2460 = DIRECTION ( 'NONE',  ( 0.000000000000000000, 0.000000000000000000, -1.000000000000000000 ) ) ;
#2461 = B_SPLINE_CURVE_WITH_KNOTS ( 'NONE', 3,
 ( #17933, #7095, #884, #18216, #18063, #24872 ),
 .UNSPECIFIED., .F., .F.,
 ( 4, 2, 4 ),
 ( 0.000000000000000000, 0.2499999999999998890, 0.5000000000000000000 ),
 .UNSPECIFIED. ) ;
#2462 = FACE_OUTER_BOUND ( 'NONE', #13499, .T. ) ;
#2463 = FACE_OUTER_BOUND ( 'NONE', #1557, .T. ) ;
#2464 = CARTESIAN_POINT ( 'NONE',  ( 0.03008364706454716778, 0.2273032555864669124, 0.000000000000000000 ) ) ;
#2465 = CIRCLE ( 'NONE', #2913, 1.988188976307287970 ) ;
#2466 = EDGE_CURVE ( 'NONE', #21409, #9119, #2876, .T. ) ;
#2467 = PLANE ( 'NONE',  #7333 ) ;
#2468 = CARTESIAN_POINT ( 'NONE',  ( -0.3702005978258633423, 0.04877294052296513721, -3.115157480314960647 ) ) ;
#2469 = CARTESIAN_POINT ( 'NONE',  ( -0.02559055118110236185, 0.000000000000000000, 0.000000000000000000 ) ) ;
#2470 = DIRECTION ( 'NONE',  ( 0.000000000000000000, 0.000000000000000000, 1.000000000000000000 ) ) ;
#2471 = LINE ( 'NONE', #4590, #14912 ) ;
#2472 = B_SPLINE_CURVE_WITH_KNOTS ( 'NONE', 3,
 ( #24519, #14078, #22838, #12092, #5167, #3034 ),
 .UNSPECIFIED., .F., .F.,
 ( 4, 2, 4 ),
 ( 0.5000000000000000000, 0.7500000000000000000, 1.000000000000000000 ),
 .UNSPECIFIED. ) ;
#2473 = ORIENTED_EDGE ( 'NONE', *, *, #20578, .F. ) ;
#2474 = CARTESIAN_POINT ( 'NONE',  ( 0.4035433070866141780, -0.7874015748031496509, 9.642888182262624280E-17 ) ) ;
#2475 = VECTOR ( 'NONE', #16821, 39.37007874015748143 ) ;
#2476 = CIRCLE ( 'NONE', #20065, 0.5118110236220472231 ) ;
#2477 = EDGE_CURVE ( 'NONE', #23407, #7809, #24171, .T. ) ;
#2478 = ORIENTED_EDGE ( 'NONE', *, *, #11220, .T. ) ;
#2479 = B_SPLINE_CURVE_WITH_KNOTS ( 'NONE', 3,
 ( #21751, #553, #23880, #10867, #19763, #9277 ),
 .UNSPECIFIED., .F., .F.,
 ( 4, 2, 4 ),
 ( 0.5000000000000000000, 0.7500000000000000000, 1.000000000000000000 ),
 .UNSPECIFIED. ) ;
#2480 = ORIENTED_EDGE ( 'NONE', *, *, #12460, .F. ) ;
#2481 = CARTESIAN_POINT ( 'NONE',  ( 0.4837521785366984406, -0.1097523286760182931, 0.2989974301281582147 ) ) ;
#2482 = CARTESIAN_POINT ( 'NONE',  ( 0.1189624676717049440, -0.3253923344978161825, 0.1377952755905510474 ) ) ;
#2483 = PRODUCT_CONTEXT ( 'NONE', #11249, 'mechanical' ) ;
#2484 = CARTESIAN_POINT ( 'NONE',  ( 0.2564944395515608710, 0.4441657790107836346, 1.766732283464566899 ) ) ;
#2485 = EDGE_CURVE ( 'NONE', #8723, #3886, #9728, .T. ) ;
#2486 = AXIS2_PLACEMENT_3D ( 'NONE', #8171, #18884, #16494 ) ;
#2487 = VERTEX_POINT ( 'NONE', #490 ) ;
#2488 = ORIENTED_EDGE ( 'NONE', *, *, #3295, .T. ) ;
#2489 = ORIENTED_EDGE ( 'NONE', *, *, #20690, .T. ) ;
#2490 = CARTESIAN_POINT ( 'NONE',  ( 0.3606853515406420185, -0.09660931395005377398, -3.115157480314960647 ) ) ;
#2491 = ORIENTED_EDGE ( 'NONE', *, *, #5759, .T. ) ;
#2492 = DIRECTION ( 'NONE',  ( -1.000000000000000000, 0.000000000000000000, 0.000000000000000000 ) ) ;
#2493 = DIRECTION ( 'NONE',  ( -1.000000000000000000, 0.000000000000000000, 0.000000000000000000 ) ) ;
#2494 = ORIENTED_EDGE ( 'NONE', *, *, #666, .T. ) ;
#2495 = CARTESIAN_POINT ( 'NONE',  ( 0.3324885138898166503, 0.04380447413659039474, 1.953740157480315043 ) ) ;
#2496 = ORIENTED_EDGE ( 'NONE', *, *, #9868, .F. ) ;
#2497 = ORIENTED_EDGE ( 'NONE', *, *, #3094, .F. ) ;
#2498 = AXIS2_PLACEMENT_3D ( 'NONE', #8653, #4425, #26293 ) ;
#2499 = CARTESIAN_POINT ( 'NONE',  ( 0.4527559054764770385, 5.549066237130534971E-17, -1.934055118110236338 ) ) ;
#2500 = AXIS2_PLACEMENT_3D ( 'NONE', #67, #6248, #14886 ) ;
#2501 = ORIENTED_EDGE ( 'NONE', *, *, #16475, .F. ) ;
#2502 = ORIENTED_EDGE ( 'NONE', *, *, #15206, .T. ) ;
#2503 = ORIENTED_EDGE ( 'NONE', *, *, #9312, .F. ) ;
#2504 = FACE_OUTER_BOUND ( 'NONE', #6759, .T. ) ;
#2506 = CARTESIAN_POINT ( 'NONE',  ( 0.3976891862754212137, 0.9951575781684135480, -0.5144425584461574941 ) ) ;
#2507 = CARTESIAN_POINT ( 'NONE',  ( 0.03532354024591842501, 0.000000000000000000, 0.000000000000000000 ) ) ;
#2508 = CARTESIAN_POINT ( 'NONE',  ( 0.7838584557816548060, 0.4717991116846240174, 0.1472977909967729537 ) ) ;
#2509 = ORIENTED_EDGE ( 'NONE', *, *, #15940, .T. ) ;
#2510 = AXIS2_PLACEMENT_3D ( 'NONE', #1761, #15064, #23256 ) ;
#2511 = DIRECTION ( 'NONE',  ( 0.000000000000000000, 1.000000000000000000, 0.000000000000000000 ) ) ;
#2512 = CARTESIAN_POINT ( 'NONE',  ( -0.3661417322834645272, 0.9448818897637796255, -1.639108661417322569E-17 ) ) ;
#2513 = LINE ( 'NONE', #7039, #22957 ) ;
#2514 = CIRCLE ( 'NONE', #22359, 0.1181102362204718703 ) ;
#2515 = CARTESIAN_POINT ( 'NONE',  ( 0.000000000000000000, 0.000000000000000000, 0.09685039370078740717 ) ) ;
#2516 = FACE_OUTER_BOUND ( 'NONE', #23288, .T. ) ;
#2517 = APPLICATION_PROTOCOL_DEFINITION ( 'draft international standard', 'automotive_design', 1998, #19177 ) ;
#2518 = ADVANCED_FACE ( 'NONE', ( #17695 ), #26322, .T. ) ;
#2519 = DIRECTION ( 'NONE',  ( 1.000000000000000000, 0.000000000000000000, 0.000000000000000000 ) ) ;
#2520 = VECTOR ( 'NONE', #6987, 39.37007874015748143 ) ;
#2521 = CARTESIAN_POINT ( 'NONE',  ( -0.5375739373539409893, 0.4296723508511047229, 0.3401574803149606252 ) ) ;
#2522 = VERTEX_POINT ( 'NONE', #2716 ) ;
#2523 = CARTESIAN_POINT ( 'NONE',  ( -0.05118110236220472370, 0.7903543307086614567, 0.000000000000000000 ) ) ;
#2524 = EDGE_LOOP ( 'NONE', ( #17900, #13744 ) ) ;
#2525 = CYLINDRICAL_SURFACE ( 'NONE', #25674, 0.1181102362204724532 ) ;
#2526 = DIRECTION ( 'NONE',  ( 1.000000000000000000, 0.000000000000000000, 0.000000000000000000 ) ) ;
#2527 = DIRECTION ( 'NONE',  ( 0.000000000000000000, 0.000000000000000000, -1.000000000000000000 ) ) ;
#2528 = CARTESIAN_POINT ( 'NONE',  ( -0.1141732283464566844, 0.7539370078740157410, 0.000000000000000000 ) ) ;
#2529 = ORIENTED_EDGE ( 'NONE', *, *, #26084, .T. ) ;
#2530 = CARTESIAN_POINT ( 'NONE',  ( 0.4954197419817712444, -0.2442565704126122561, 0.9202755905511811330 ) ) ;
#2531 = DIRECTION ( 'NONE',  ( -0.7071067818211409506, 0.7071067805519539728, 8.659560554583403090E-17 ) ) ;
#2532 = EDGE_LOOP ( 'NONE', ( #7536, #5991 ) ) ;
#2533 = CARTESIAN_POINT ( 'NONE',  ( 0.000000000000000000, 0.000000000000000000, 0.4488188976377953110 ) ) ;
#2534 = CIRCLE ( 'NONE', #18307, 0.6212598425196850238 ) ;
#2535 = CARTESIAN_POINT ( 'NONE',  ( -0.6299212598425196763, -0.4526313213353582721, -0.9943460912301771426 ) ) ;
#2536 = DIRECTION ( 'NONE',  ( 1.000000000000000000, 0.000000000000000000, 0.000000000000000000 ) ) ;
#2537 = FACE_OUTER_BOUND ( 'NONE', #20320, .T. ) ;
#2538 = CARTESIAN_POINT ( 'NONE',  ( 0.3048711895203580768, -0.6348424542976517371, 0.3281099440179709448 ) ) ;
#2539 = ADVANCED_FACE ( 'NONE', ( #2271, #12732 ), #18948, .T. ) ;
#2540 = AXIS2_PLACEMENT_3D ( 'NONE', #18666, #12049, #20945 ) ;
#2541 = DIRECTION ( 'NONE',  ( 0.000000000000000000, 0.000000000000000000, 1.000000000000000000 ) ) ;
#2542 = FACE_OUTER_BOUND ( 'NONE', #3536, .T. ) ;
#2543 = CARTESIAN_POINT ( 'NONE',  ( 1.692913385826771533, 0.4724409448818898127, 0.1181102362204723144 ) ) ;
#2544 = CARTESIAN_POINT ( 'NONE',  ( 0.1839420097223035677, -0.5417097841048799101, 0.9399606299212598381 ) ) ;
#2545 = EDGE_CURVE ( 'NONE', #11128, #16194, #21500, .T. ) ;
#2546 = FACE_OUTER_BOUND ( 'NONE', #22789, .T. ) ;
#2547 = PLANE ( 'NONE',  #12830 ) ;
#2548 = ORIENTED_EDGE ( 'NONE', *, *, #8868, .F. ) ;
#2549 = VECTOR ( 'NONE', #10663, 39.37007874015748143 ) ;
#2550 = EDGE_LOOP ( 'NONE', ( #23716, #23135, #18608, #25264 ) ) ;
#2551 = ORIENTED_EDGE ( 'NONE', *, *, #23911, .F. ) ;
#2552 = CIRCLE ( 'NONE', #3434, 0.3937007873768824662 ) ;
#2553 = DIRECTION ( 'NONE',  ( -0.2036417511401758251, 0.9790454724845842893, -1.198984999999999602E-16 ) ) ;
#2554 = DIRECTION ( 'NONE',  ( 1.000000000000000000, 0.000000000000000000, 0.000000000000000000 ) ) ;
#2555 = ORIENTED_EDGE ( 'NONE', *, *, #16773, .T. ) ;
#2556 = SPHERICAL_SURFACE ( 'NONE', #2498, 0.1299232283464566984 ) ;
#2557 = ORIENTED_EDGE ( 'NONE', *, *, #12567, .F. ) ;
#2558 = CARTESIAN_POINT ( 'NONE',  ( 0.5869493968219645641, 0.2133897621573074832, -0.3696019098714952711 ) ) ;
#2559 = EDGE_CURVE ( 'NONE', #27334, #51, #15612, .T. ) ;
#2560 = CARTESIAN_POINT ( 'NONE',  ( 0.1525037638700915965, 0.2637554987713723320, -0.4194810972668293614 ) ) ;
#2561 = CARTESIAN_POINT ( 'NONE',  ( 3.387491338582676985E-16, -0.6299212598425196763, 0.000000000000000000 ) ) ;
#2562 = B_SPLINE_CURVE_WITH_KNOTS ( 'NONE', 3,
 ( #5700, #12044, #18522, #14313 ),
 .UNSPECIFIED., .F., .F.,
 ( 4, 4 ),
 ( 0.000000000000000000, 0.4421524820080139917 ),
 .UNSPECIFIED. ) ;
#2563 = CARTESIAN_POINT ( 'NONE',  ( -0.3268074212154853941, -0.1882834141668338901, 0.1992142436757342316 ) ) ;
#2564 = EDGE_CURVE ( 'NONE', #3577, #11261, #6383, .T. ) ;
#2565 = ( GEOMETRIC_REPRESENTATION_CONTEXT ( 3 ) GLOBAL_UNCERTAINTY_ASSIGNED_CONTEXT ( ( #14423 ) ) GLOBAL_UNIT_ASSIGNED_CONTEXT ( ( #309, #11554, #24143 ) ) REPRESENTATION_CONTEXT ( 'NONE', 'WORKASPACE' ) ) ;
#2566 = PRODUCT_DEFINITION ( 'UNKNOWN', '', #22916, #5726 ) ;
#2567 = VERTEX_POINT ( 'NONE', #17258 ) ;
#2568 = FACE_OUTER_BOUND ( 'NONE', #25010, .T. ) ;
#2569 = CARTESIAN_POINT ( 'NONE',  ( -0.4270824798167728864, 0.2466292688015120915, -1.550196850393700920 ) ) ;
#2570 = EDGE_CURVE ( 'NONE', #12477, #20698, #19211, .T. ) ;
#2571 = DIRECTION ( 'NONE',  ( 0.000000000000000000, 0.000000000000000000, 1.000000000000000000 ) ) ;
#2572 = AXIS2_PLACEMENT_3D ( 'NONE', #1077, #5152, #10509 ) ;
#2573 = CARTESIAN_POINT ( 'NONE',  ( -0.3362148458988422073, 0.4382482975805319092, 0.9202755905511811330 ) ) ;
#2574 = EDGE_CURVE ( 'NONE', #18722, #496, #24781, .T. ) ;
#2575 = CARTESIAN_POINT ( 'NONE',  ( 0.3082037322259243428, 0.3663931537943041494, 0.1920935997044755372 ) ) ;
#2576 = APPLICATION_CONTEXT ( 'automotive_design' ) ;
#2577 = CARTESIAN_POINT ( 'NONE',  ( 0.03001016326913580681, 0.4585215200179055817, -1.928289503579156516 ) ) ;
#2578 = CARTESIAN_POINT ( 'NONE',  ( -0.6305589872448129629, -0.06986321629937303213, -0.08121850359745433345 ) ) ;
#2579 = FACE_OUTER_BOUND ( 'NONE', #25724, .T. ) ;
#2580 = EDGE_LOOP ( 'NONE', ( #27237, #13937 ) ) ;
#2581 = TOROIDAL_SURFACE ( 'NONE', #9808, 0.5610236220472440971, 0.1003937007874015908 ) ;
#2583 = DIRECTION ( 'NONE',  ( 0.4999999999999996114, 0.8660254037844389297, 0.000000000000000000 ) ) ;
#2582 = LINE ( 'NONE', #17062, #18450 ) ;
#2584 = AXIS2_PLACEMENT_3D ( 'NONE', #16426, #25324, #5986 ) ;
#2585 = DIRECTION ( 'NONE',  ( 0.000000000000000000, 0.000000000000000000, -1.000000000000000000 ) ) ;
#2586 = CIRCLE ( 'NONE', #7558, 0.6881889763779527325 ) ;
#2587 = PRODUCT_DEFINITION_SHAPE ( 'NONE', 'NONE',  #27886 ) ;
#2588 = DIRECTION ( 'NONE',  ( 0.000000000000000000, 0.000000000000000000, 1.000000000000000000 ) ) ;
#2589 = CARTESIAN_POINT ( 'NONE',  ( 0.000000000000000000, 0.000000000000000000, -3.110236220451535694 ) ) ;
#2590 = DIRECTION ( 'NONE',  ( 1.000000000000000000, 0.000000000000000000, 0.000000000000000000 ) ) ;
#2591 = VERTEX_POINT ( 'NONE', #19374 ) ;
#2592 = CARTESIAN_POINT ( 'NONE',  ( -0.4527559054764770385, 0.02963280468031418563, -1.934055118110236338 ) ) ;
#2593 = CONICAL_SURFACE ( 'NONE', #18365, 0.4863540308881693086, 1.365720138124999927 ) ;
#2594 = DIRECTION ( 'NONE',  ( 0.000000000000000000, 0.000000000000000000, -1.000000000000000000 ) ) ;
#2595 = ADVANCED_FACE ( 'NONE', ( #26012 ), #4331, .F. ) ;
#2596 = CARTESIAN_POINT ( 'NONE',  ( -0.6869867706933208140, 0.7419671345971732279, -0.1783180911161240390 ) ) ;
#2597 = EDGE_CURVE ( 'NONE', #27102, #1802, #532, .T. ) ;
#2598 = LINE ( 'NONE', #8828, #8704 ) ;
#2599 = CARTESIAN_POINT ( 'NONE',  ( 0.2993674444872233553, -0.2296683860596848981, -3.100567304031763172 ) ) ;
#2600 = DIRECTION ( 'NONE',  ( 0.000000000000000000, 0.000000000000000000, 1.000000000000000000 ) ) ;
#2601 = CARTESIAN_POINT ( 'NONE',  ( -0.2243804351489621651, 0.2666304421170154759, 0.1166443193998331490 ) ) ;
#2602 = CARTESIAN_POINT ( 'NONE',  ( 0.6339803004464725777, 0.1124719464480360975, 0.1183902030413380158 ) ) ;
#2603 = B_SPLINE_CURVE_WITH_KNOTS ( 'NONE', 2,
 ( #11290, #26521, #13679 ),
 .UNSPECIFIED., .F., .F.,
 ( 3, 3 ),
 ( 0.000000000000000000, 1.000000000000000000 ),
 .UNSPECIFIED. ) ;
#2604 = ADVANCED_FACE ( 'NONE', ( #15156 ), #8024, .T. ) ;
#2605 = AXIS2_PLACEMENT_3D ( 'NONE', #9872, #10429, #27399 ) ;
#2606 = ORIENTED_EDGE ( 'NONE', *, *, #23570, .F. ) ;
#2607 = CARTESIAN_POINT ( 'NONE',  ( 0.000000000000000000, 0.000000000000000000, -4.015748031496062964 ) ) ;
#2608 = CIRCLE ( 'NONE', #7135, 0.09842519685039370636 ) ;
#2609 = DIRECTION ( 'NONE',  ( 1.000000000000000000, 0.000000000000000000, 0.000000000000000000 ) ) ;
#2610 = AXIS2_PLACEMENT_3D ( 'NONE', #8395, #23235, #3870 ) ;
#2611 = ORIENTED_EDGE ( 'NONE', *, *, #15702, .F. ) ;
#2612 = CIRCLE ( 'NONE', #6255, 0.4807043897637795493 ) ;
#2613 = DIRECTION ( 'NONE',  ( 1.000000000000000000, 0.000000000000000000, 0.000000000000000000 ) ) ;
#2614 = CARTESIAN_POINT ( 'NONE',  ( -0.4984899526255159308, 0.1339654526248284516, 1.766732283464566899 ) ) ;
#2615 = CARTESIAN_POINT ( 'NONE',  ( -0.5085118447801413311, 0.06699507805369032953, 1.747047244094488194 ) ) ;
#2616 = FILL_AREA_STYLE ('',( #21575 ) ) ;
#2617 = ADVANCED_FACE ( 'NONE', ( #25802, #23284 ), #27795, .T. ) ;
#2618 = ORIENTED_EDGE ( 'NONE', *, *, #8797, .T. ) ;
#2619 = EDGE_LOOP ( 'NONE', ( #16072, #19591, #4603, #3997 ) ) ;
#2621 = CARTESIAN_POINT ( 'NONE',  ( -0.3726024258163779246, -0.02438677169354843896, -3.115157480314960647 ) ) ;
#2620 = CARTESIAN_POINT ( 'NONE',  ( -0.6512499169089656093, 0.1155267097728523984, 0.1616495878834900424 ) ) ;
#2622 = CARTESIAN_POINT ( 'NONE',  ( 0.000000000000000000, 0.000000000000000000, 0.2574803149606298969 ) ) ;
#2623 = ORIENTED_EDGE ( 'NONE', *, *, #25477, .T. ) ;
#2624 = CARTESIAN_POINT ( 'NONE',  ( 0.1755067523729419432, -0.3028750839302634112, 0.5245950337139047015 ) ) ;
#2625 = DIRECTION ( 'NONE',  ( -0.9790454724845842893, -0.2036417511401760472, 2.493892000000000781E-17 ) ) ;
#2626 = CARTESIAN_POINT ( 'NONE',  ( 0.2041304421298504035, -0.2660793235464293249, 1.953740157480315043 ) ) ;
#2627 = ORIENTED_EDGE ( 'NONE', *, *, #4655, .T. ) ;
#2628 = VERTEX_POINT ( 'NONE', #21147 ) ;
#2629 = VECTOR ( 'NONE', #24396, 39.37007874015748854 ) ;
#2630 = CARTESIAN_POINT ( 'NONE',  ( -0.2362204724409449064, 0.9448818897637796255, 0.1308464566929133654 ) ) ;
#2631 = CARTESIAN_POINT ( 'NONE',  ( -0.6707652279343464530, -0.1538768215239710857, 0.1322834645669291320 ) ) ;
#2632 = AXIS2_PLACEMENT_3D ( 'NONE', #14783, #10215, #18829 ) ;
#2633 = EDGE_LOOP ( 'NONE', ( #23889, #12887 ) ) ;
#2634 = EDGE_LOOP ( 'NONE', ( #21709, #12483, #8120, #17743, #16275, #6478 ) ) ;
#2635 = ORIENTED_EDGE ( 'NONE', *, *, #16037, .F. ) ;
#2636 = CARTESIAN_POINT ( 'NONE',  ( -0.4167985568850881561, 0.07349283109919310664, 0.1377952755905511861 ) ) ;
#2637 = CARTESIAN_POINT ( 'NONE',  ( 0.000000000000000000, 0.000000000000000000, 0.1771653543307086520 ) ) ;
#2638 = CARTESIAN_POINT ( 'NONE',  ( 0.06881018027183069541, 0.1968503937007874127, -3.233009657539146708 ) ) ;
#2639 = AXIS2_PLACEMENT_3D ( 'NONE', #27845, #16966, #4383 ) ;
#2640 = CARTESIAN_POINT ( 'NONE',  ( -6.132876883919029269E-17, -0.5007874015748031704, 0.2574803149606298969 ) ) ;
#2641 = ORIENTED_EDGE ( 'NONE', *, *, #6158, .F. ) ;
#2642 = EDGE_CURVE ( 'NONE', #5602, #25182, #2, .T. ) ;
#2643 = ORIENTED_EDGE ( 'NONE', *, *, #3133, .T. ) ;
#2644 = CARTESIAN_POINT ( 'NONE',  ( 0.1638952246732497953, 0.2749627978706433162, -0.4762495361032464958 ) ) ;
#2645 = CARTESIAN_POINT ( 'NONE',  ( -0.02319089060378104472, -0.3543307086614173596, 1.953740157480315043 ) ) ;
#2646 = EDGE_CURVE ( 'NONE', #11007, #6574, #1695, .T. ) ;
#2647 = AXIS2_PLACEMENT_3D ( 'NONE', #2061, #19434, #125 ) ;
#2648 = CARTESIAN_POINT ( 'NONE',  ( -4.618943439303797186E-17, -0.3771653543307086909, 0.2755905511811023723 ) ) ;
#2649 = AXIS2_PLACEMENT_3D ( 'NONE', #1515, #3620, #10126 ) ;
#2650 = CYLINDRICAL_SURFACE ( 'NONE', #4021, 0.3149606299212598381 ) ;
#2651 = AXIS2_PLACEMENT_3D ( 'NONE', #5903, #1649, #10254 ) ;
#2652 = DIRECTION ( 'NONE',  ( 0.000000000000000000, 0.000000000000000000, 1.000000000000000000 ) ) ;
#2653 = DIRECTION ( 'NONE',  ( -0.000000000000000000, -0.000000000000000000, -1.000000000000000000 ) ) ;
#2654 = CARTESIAN_POINT ( 'NONE',  ( 0.4842519685039370358, 5.930376232091513698E-17, -0.2480314960629921295 ) ) ;
#2655 = VERTEX_POINT ( 'NONE', #1791 ) ;
#2656 = AXIS2_PLACEMENT_3D ( 'NONE', #9060, #23786, #89 ) ;
#2657 = CARTESIAN_POINT ( 'NONE',  ( 0.3751294191746888940, 0.2999672986753446624, 0.2194422276300426189 ) ) ;
#2658 = CARTESIAN_POINT ( 'NONE',  ( -0.4897507849295944515, 0.08575075074566133881, 0.1140743250927050007 ) ) ;
#2659 = ORIENTED_EDGE ( 'NONE', *, *, #23278, .F. ) ;
#2660 = CARTESIAN_POINT ( 'NONE',  ( 0.4527559054764771496, 0.000000000000000000, -1.934055118110236338 ) ) ;
#2661 = CARTESIAN_POINT ( 'NONE',  ( 0.6864238947237005783, -0.1574599019770832331, 0.3281099440179374715 ) ) ;
#2662 = EDGE_LOOP ( 'NONE', ( #10373, #24245, #4890, #12960, #14300, #21059 ) ) ;
#2663 = CARTESIAN_POINT ( 'NONE',  ( -0.07214854559198104200, 0.5476281405333119912, 0.9399606299212598381 ) ) ;
#2664 = LINE ( 'NONE', #17778, #15369 ) ;
#2665 = ORIENTED_EDGE ( 'NONE', *, *, #21755, .F. ) ;
#2666 = ADVANCED_FACE ( 'NONE', ( #16628 ), #15675, .T. ) ;
#2667 = CARTESIAN_POINT ( 'NONE',  ( 0.3988311005573134116, 0.4763376377694984454, 0.09685039370078740717 ) ) ;
#2668 = AXIS2_PLACEMENT_3D ( 'NONE', #15432, #4402, #12870 ) ;
#2669 = CARTESIAN_POINT ( 'NONE',  ( 0.2274877609439496517, -0.4708572476046440358, 0.3331434174476592402 ) ) ;
#2670 = CIRCLE ( 'NONE', #22528, 0.4980314960629921295 ) ;
#2671 = DIRECTION ( 'NONE',  ( 0.000000000000000000, -1.000000000000000000, 0.000000000000000000 ) ) ;
#2672 = DIRECTION ( 'NONE',  ( 0.000000000000000000, -0.5749917231862786693, 0.8181592254978695689 ) ) ;
#2673 = CARTESIAN_POINT ( 'NONE',  ( 0.6299212598425196763, -1.895600393700787470E-35, 0.000000000000000000 ) ) ;
#2674 = ADVANCED_FACE ( 'NONE', ( #8431 ), #10402, .T. ) ;
#2675 = ADVANCED_FACE ( 'NONE', ( #18435, #27363 ), #8013, .T. ) ;
#2676 = DIRECTION ( 'NONE',  ( 0.000000000000000000, 1.000000000000000000, 0.000000000000000000 ) ) ;
#2677 = CARTESIAN_POINT ( 'NONE',  ( 0.0001724821237276073489, 0.3771653543307085243, 0.07637549214372833795 ) ) ;
#2678 = CARTESIAN_POINT ( 'NONE',  ( -0.2529800193559321730, -0.5131133041954082374, 0.9399606299212598381 ) ) ;
#2679 = CARTESIAN_POINT ( 'NONE',  ( 0.2146455952155474356, -0.4472013107345719218, 0.2989974300902882298 ) ) ;
#2680 = CARTESIAN_POINT ( 'NONE',  ( -0.1285103288269285327, -0.3545966721392122545, 0.07637795275590551769 ) ) ;
#2681 = DIRECTION ( 'NONE',  ( 0.000000000000000000, 1.000000000000000000, 0.000000000000000000 ) ) ;
#2682 = CARTESIAN_POINT ( 'NONE',  ( -0.4887136534522864562, -0.1122103150216818279, 0.1643955689363730821 ) ) ;
#2683 = TOROIDAL_SURFACE ( 'NONE', #4951, 0.5610236220472440971, 0.1003937007874015908 ) ;
#2684 = TOROIDAL_SURFACE ( 'NONE', #9004, 0.5610236220472440971, 0.1003937007874015908 ) ;
#2685 = ORIENTED_EDGE ( 'NONE', *, *, #23444, .T. ) ;
#2686 = CIRCLE ( 'NONE', #13519, 0.07874015748031489015 ) ;
#2687 = DIRECTION ( 'NONE',  ( 0.000000000000000000, -1.000000000000000000, 0.000000000000000000 ) ) ;
#2688 = CARTESIAN_POINT ( 'NONE',  ( 0.000000000000000000, 0.000000000000000000, 0.09685039370078740717 ) ) ;
#2689 = ORIENTED_EDGE ( 'NONE', *, *, #22485, .T. ) ;
#2690 = CARTESIAN_POINT ( 'NONE',  ( 0.1120675189988346587, -0.4694218845611126678, -0.3846748511993476338 ) ) ;
#2691 = CARTESIAN_POINT ( 'NONE',  ( -0.4690668203699855932, 0.08212126673558327317, 0.1212655228837342947 ) ) ;
#2692 = CARTESIAN_POINT ( 'NONE',  ( 0.7430739993161732393, 0.4432762660064943905, -0.3627962913661458288 ) ) ;
#2693 = AXIS2_PLACEMENT_3D ( 'NONE', #16720, #10352, #2021 ) ;
#2694 = DIRECTION ( 'NONE',  ( 1.000000000000000000, 0.000000000000000000, 0.000000000000000000 ) ) ;
#2695 = AXIS2_PLACEMENT_3D ( 'NONE', #25972, #417, #8999 ) ;
#2696 = DIRECTION ( 'NONE',  ( 1.000000000000000000, 0.000000000000000000, 0.000000000000000000 ) ) ;
#2697 = ORIENTED_EDGE ( 'NONE', *, *, #12178, .T. ) ;
#2698 = CARTESIAN_POINT ( 'NONE',  ( 0.02564049093248907743, 0.3139791838537054902, -3.643473821106772981 ) ) ;
#2699 = CARTESIAN_POINT ( 'NONE',  ( -0.09842519685039370636, -1.570035826771653483E-17, -0.09092130223458683158 ) ) ;
#2700 = CARTESIAN_POINT ( 'NONE',  ( 0.06699507805605696420, 0.5085118447796661556, -1.550196850393700920 ) ) ;
#2701 = CARTESIAN_POINT ( 'NONE',  ( 0.3645739570812638330, -0.2796934465393868807, -1.928289503579156072 ) ) ;
#2702 = VERTEX_POINT ( 'NONE', #7731 ) ;
#2703 = CARTESIAN_POINT ( 'NONE',  ( 0.1188866373884749916, -0.4438564651657395665, -1.928289503579163178 ) ) ;
#2704 = AXIS2_PLACEMENT_3D ( 'NONE', #14804, #21278, #1355 ) ;
#2705 = CARTESIAN_POINT ( 'NONE',  ( -0.03607471876262472593, 0.5511811023622047445, 0.9202755905511811330 ) ) ;
#2706 = DIRECTION ( 'NONE',  ( -1.000000000000000000, 0.000000000000000000, 0.000000000000000000 ) ) ;
#2707 = MANIFOLD_SOLID_BREP ( 'Index Plate', #6943 ) ;
#2708 = CARTESIAN_POINT ( 'NONE',  ( 0.3713752547280854133, 0.06583429795695137920, 0.1992142436757342316 ) ) ;
#2709 = CARTESIAN_POINT ( 'NONE',  ( 0.1477428134820460426, 0.4351030398461616100, -1.928289503579165842 ) ) ;
#2710 = CARTESIAN_POINT ( 'NONE',  ( -0.1968503937007874127, 0.07874015748031495954, -0.04546065111729338803 ) ) ;
#2711 = CARTESIAN_POINT ( 'NONE',  ( -0.6262477747318130339, -0.09467419725595611901, 0.07480744568936535666 ) ) ;
#2712 = DIRECTION ( 'NONE',  ( 0.7071067818211401734, 8.659560570126452765E-17, -0.7071067805519547500 ) ) ;
#2713 = EDGE_CURVE ( 'NONE', #15744, #16084, #3962, .T. ) ;
#2714 = CARTESIAN_POINT ( 'NONE',  ( 0.2305483297598421022, -0.4797636960996590760, 0.1322818204150988386 ) ) ;
#2715 = AXIS2_PLACEMENT_3D ( 'NONE', #11396, #22136, #24804 ) ;
#2716 = CARTESIAN_POINT ( 'NONE',  ( -0.3020979083623086536, 0.3591256245825952265, 0.1992125984251968684 ) ) ;
#2717 = CARTESIAN_POINT ( 'NONE',  ( 0.4858607088160724063, -0.2805118110236220486, 0.1771653543307086520 ) ) ;
#2718 = ORIENTED_EDGE ( 'NONE', *, *, #10592, .T. ) ;
#2719 = CARTESIAN_POINT ( 'NONE',  ( -0.09842519685039370636, 2.800920866141732248E-17, 0.09092130223458683158 ) ) ;
#2720 = EDGE_CURVE ( 'NONE', #5602, #19729, #7100, .T. ) ;
#2721 = ORIENTED_EDGE ( 'NONE', *, *, #27018, .T. ) ;
#2722 = CARTESIAN_POINT ( 'NONE',  ( -0.6722178168900768691, 0.05124196228576535783, 0.07772299437287735757 ) ) ;
#2723 = EDGE_LOOP ( 'NONE', ( #26638, #22078, #16466, #23009 ) ) ;
#2724 = STYLED_ITEM ( 'NONE', ( #17058 ), #12201 ) ;
#2725 = CARTESIAN_POINT ( 'NONE',  ( 0.2423050875943944527, 0.2890362931940642088, 0.07637549214372835182 ) ) ;
#2726 = ORIENTED_EDGE ( 'NONE', *, *, #25744, .T. ) ;
#2727 = DIRECTION ( 'NONE',  ( -1.000000000000000000, 0.000000000000000000, 0.000000000000000000 ) ) ;
#2728 = ADVANCED_FACE ( 'NONE', ( #4189 ), #21424, .T. ) ;
#2729 = EDGE_CURVE ( 'NONE', #12355, #25409, #17051, .T. ) ;
#2730 = CARTESIAN_POINT ( 'NONE',  ( -0.4858607088160732390, -0.2805118110236220486, 0.1771653543307086520 ) ) ;
#2731 = CARTESIAN_POINT ( 'NONE',  ( -0.3355349563089150000, 0.1402003033445870239, 0.07874015748031495954 ) ) ;
#2732 = DIRECTION ( 'NONE',  ( 0.000000000000000000, 0.000000000000000000, -1.000000000000000000 ) ) ;
#2733 = CARTESIAN_POINT ( 'NONE',  ( 0.1886891683788904650, 0.3267488823401754061, -3.100567304031762284 ) ) ;
#2734 = CARTESIAN_POINT ( 'NONE',  ( 0.5949363243629232079, -0.1357903337134992172, 0.2362204724409449064 ) ) ;
#2735 = CARTESIAN_POINT ( 'NONE',  ( 0.2705157149885996093, 0.7122990885670630323, 0.000000000000000000 ) ) ;
#2736 = CARTESIAN_POINT ( 'NONE',  ( 0.1493472610806836076, 0.2566546340585424968, 0.4057060197093078080 ) ) ;
#2737 = EDGE_LOOP ( 'NONE', ( #14308, #15198, #18817, #27078 ) ) ;
#2738 = DIRECTION ( 'NONE',  ( -1.000000000000000000, 0.000000000000000000, 0.000000000000000000 ) ) ;
#2739 = AXIS2_PLACEMENT_3D ( 'NONE', #23817, #4184, #16905 ) ;
#2740 = CIRCLE ( 'NONE', #24408, 0.3937007874015748254 ) ;
#2741 = CIRCLE ( 'NONE', #978, 0.3831516066089791228 ) ;
#2742 = VERTEX_POINT ( 'NONE', #10957 ) ;
#2743 = FACE_BOUND ( 'NONE', #15245, .T. ) ;
#2744 = CARTESIAN_POINT ( 'NONE',  ( 0.000000000000000000, 0.000000000000000000, -0.4724409448841456749 ) ) ;
#2745 = CARTESIAN_POINT ( 'NONE',  ( -0.2268096725222598919, -0.4600326175560532915, 1.747047244094488194 ) ) ;
#2746 = CYLINDRICAL_SURFACE ( 'NONE', #14802, 0.4692913385826771866 ) ;
#2747 = VERTEX_POINT ( 'NONE', #19151 ) ;
#2748 = CARTESIAN_POINT ( 'NONE',  ( 0.2462256503455911016, 0.2807137536170354331, -3.115157480314960647 ) ) ;
#2749 = FACE_OUTER_BOUND ( 'NONE', #15667, .T. ) ;
#2750 = LINE ( 'NONE', #4347, #6018 ) ;
#2751 = CARTESIAN_POINT ( 'NONE',  ( 0.5021077788561401078, -0.1139291307083168392, 0.1473214333284243727 ) ) ;
#2752 = EDGE_CURVE ( 'NONE', #16609, #27306, #2586, .T. ) ;
#2753 = B_SPLINE_CURVE_WITH_KNOTS ( 'NONE', 3,
 ( #8016, #16623, #21003, #1648, #10252, #8157, #16767, #11169, #21110, #18984 ),
 .UNSPECIFIED., .F., .F.,
 ( 4, 2, 2, 2, 4 ),
 ( 0.000000000000000000, 0.2500000000000000000, 0.5000000000000000000, 0.7500000000000000000, 1.000000000000000000 ),
 .UNSPECIFIED. ) ;
#2754 = VERTEX_POINT ( 'NONE', #17045 ) ;
#2755 = CARTESIAN_POINT ( 'NONE',  ( -0.3346456692913385988, -0.02190250779246036283, 1.953740157480315043 ) ) ;
#2756 = VERTEX_POINT ( 'NONE', #6727 ) ;
#2757 = ORIENTED_EDGE ( 'NONE', *, *, #17561, .T. ) ;
#2758 = EDGE_LOOP ( 'NONE', ( #12853, #9072, #23845, #6887 ) ) ;
#2759 = DIRECTION ( 'NONE',  ( 0.000000000000000000, 0.000000000000000000, -1.000000000000000000 ) ) ;
#2760 = EDGE_CURVE ( 'NONE', #13081, #6094, #26969, .T. ) ;
#2761 = ORIENTED_EDGE ( 'NONE', *, *, #2947, .F. ) ;
#2762 = ORIENTED_EDGE ( 'NONE', *, *, #8060, .F. ) ;
#2763 = CARTESIAN_POINT ( 'NONE',  ( 0.06294381634853177254, 0.1968503937007874127, -3.596635957034346021 ) ) ;
#2764 = AXIS2_PLACEMENT_3D ( 'NONE', #194, #11024, #26267 ) ;
#2765 = CARTESIAN_POINT ( 'NONE',  ( -0.03794311743615354227, 0.6358669483106004217, -0.5146366652951276377 ) ) ;
#2766 = CARTESIAN_POINT ( 'NONE',  ( 0.000000000000000000, 0.000000000000000000, -0.01377952755905511792 ) ) ;
#2767 = CARTESIAN_POINT ( 'NONE',  ( 0.000000000000000000, 0.000000000000000000, 1.747047244094488194 ) ) ;
#2768 = EDGE_CURVE ( 'NONE', #7482, #18177, #8831, .T. ) ;
#2769 = FACE_OUTER_BOUND ( 'NONE', #11806, .T. ) ;
#2770 = CARTESIAN_POINT ( 'NONE',  ( -0.1570220809524502104, -0.3184841198566448206, 1.953740157480315043 ) ) ;
#2771 = CARTESIAN_POINT ( 'NONE',  ( 0.6707652279343347956, -0.1538768215240155779, 0.3401574803149606252 ) ) ;
#2772 = CONICAL_SURFACE ( 'NONE', #11805, 1.988188976307287970, 0.7853981642948970610 ) ;
#2773 = CARTESIAN_POINT ( 'NONE',  ( 0.1490609433615242285, 0.2393035190771452825, -0.4144858534716441278 ) ) ;
#2774 = DIRECTION ( 'NONE',  ( 0.000000000000000000, 0.000000000000000000, -1.000000000000000000 ) ) ;
#2775 = CARTESIAN_POINT ( 'NONE',  ( 0.000000000000000000, 0.000000000000000000, 0.09685039370078740717 ) ) ;
#2776 = DIRECTION ( 'NONE',  ( -0.000000000000000000, 1.000000000000000000, -0.000000000000000000 ) ) ;
#2777 = CARTESIAN_POINT ( 'NONE',  ( 0.3121994997598427912, 0.4069448477556012467, 1.766732283464566899 ) ) ;
#2778 = EDGE_CURVE ( 'NONE', #26868, #27250, #21542, .T. ) ;
#2779 = CIRCLE ( 'NONE', #17251, 0.3543307086367249448 ) ;
#2780 = CARTESIAN_POINT ( 'NONE',  ( 0.4211031283186273955, -0.2438048970108675773, 0.1827409795176048457 ) ) ;
#2781 = EDGE_LOOP ( 'NONE', ( #16201, #23225, #21886, #15230 ) ) ;
#2782 = LINE ( 'NONE', #11011, #8118 ) ;
#2783 = VECTOR ( 'NONE', #20849, 39.37007874015748854 ) ;
#2784 = EDGE_CURVE ( 'NONE', #13707, #10268, #25934, .T. ) ;
#2785 = ORIENTED_EDGE ( 'NONE', *, *, #8151, .T. ) ;
#2786 = CARTESIAN_POINT ( 'NONE',  ( -0.03937007874015747977, 0.000000000000000000, 0.000000000000000000 ) ) ;
#2787 = ORIENTED_EDGE ( 'NONE', *, *, #19782, .T. ) ;
#2788 = CARTESIAN_POINT ( 'NONE',  ( -0.2647715730835492609, -0.5498038367121063086, 0.1062972440944881941 ) ) ;
#2789 = ORIENTED_EDGE ( 'NONE', *, *, #5062, .T. ) ;
#2790 = CARTESIAN_POINT ( 'NONE',  ( 0.03607471876262387245, -0.5511811023622048555, 0.9399606299212598381 ) ) ;
#2791 = VERTEX_POINT ( 'NONE', #12929 ) ;
#2792 = CARTESIAN_POINT ( 'NONE',  ( 0.000000000000000000, 0.000000000000000000, 1.747047244094488194 ) ) ;
#2793 = ORIENTED_EDGE ( 'NONE', *, *, #23347, .F. ) ;
#2794 = CIRCLE ( 'NONE', #3231, 0.7874015748031496509 ) ;
#2795 = CARTESIAN_POINT ( 'NONE',  ( 0.000000000000000000, 0.000000000000000000, 0.3401574803149606252 ) ) ;
#2796 = CARTESIAN_POINT ( 'NONE',  ( 0.000000000000000000, 0.1968503937007874127, -0.3937007874015748254 ) ) ;
#2797 = CARTESIAN_POINT ( 'NONE',  ( -0.1580799066051627177, -0.4326553680327468454, 0.1771653543307088186 ) ) ;
#2798 = DIRECTION ( 'NONE',  ( -0.2036417511401761582, 0.4895227362422917006, -0.8478782506317886769 ) ) ;
#2799 = AXIS2_PLACEMENT_3D ( 'NONE', #20368, #22920, #1028 ) ;
#2800 = CARTESIAN_POINT ( 'NONE',  ( 0.1516263115863346334, 0.4909405214979283838, 0.05579628926458630317 ) ) ;
#2801 = CARTESIAN_POINT ( 'NONE',  ( -0.3239425792934415571, -0.08676778863010886633, 1.953740157480315043 ) ) ;
#2802 = VERTEX_POINT ( 'NONE', #126 ) ;
#2803 = DIRECTION ( 'NONE',  ( -1.000000000000000000, 0.000000000000000000, 0.000000000000000000 ) ) ;
#2804 = CARTESIAN_POINT ( 'NONE',  ( 0.4065144339881236468, -0.2344790234878192936, 0.07637549214372854611 ) ) ;
#2805 = CARTESIAN_POINT ( 'NONE',  ( 0.7165354330708662012, 0.000000000000000000, -3.278217716535432842E-17 ) ) ;
#2806 = CARTESIAN_POINT ( 'NONE',  ( -0.1339654526248285349, -0.4984899526255157087, 1.766732283464566677 ) ) ;
#2807 = DIRECTION ( 'NONE',  ( 0.000000000000000000, 0.000000000000000000, 1.000000000000000000 ) ) ;
#2808 = PRODUCT_DEFINITION_SHAPE ( 'NONE', 'NONE',  #27890 ) ;
#2809 = CARTESIAN_POINT ( 'NONE',  ( 0.3574961452116665606, 0.02345921195965534889, -3.115157480314960647 ) ) ;
#2810 = DIRECTION ( 'NONE',  ( 0.000000000000000000, 0.000000000000000000, 1.000000000000000000 ) ) ;
#2811 = AXIS2_PLACEMENT_3D ( 'NONE', #14470, #19390, #16714 ) ;
#2812 = EDGE_CURVE ( 'NONE', #2225, #7703, #23380, .T. ) ;
#2813 = AXIS2_PLACEMENT_3D ( 'NONE', #9732, #3355, #3801 ) ;
#2814 = ORIENTED_EDGE ( 'NONE', *, *, #17711, .T. ) ;
#2815 = CIRCLE ( 'NONE', #9598, 0.1298643763538142593 ) ;
#2816 = EDGE_CURVE ( 'NONE', #23841, #11054, #503, .T. ) ;
#2817 = ORIENTED_EDGE ( 'NONE', *, *, #21955, .T. ) ;
#2818 = CARTESIAN_POINT ( 'NONE',  ( 0.4130706566799093316, 0.3346769814300175616, 0.5796775359605756961 ) ) ;
#2819 = CARTESIAN_POINT ( 'NONE',  ( 0.000000000000000000, 0.000000000000000000, 0.1377952755905511861 ) ) ;
#2820 = EDGE_LOOP ( 'NONE', ( #12186, #18779 ) ) ;
#2821 = FACE_OUTER_BOUND ( 'NONE', #2634, .T. ) ;
#2822 = ORIENTED_EDGE ( 'NONE', *, *, #16341, .F. ) ;
#2823 = DIRECTION ( 'NONE',  ( 0.000000000000000000, 0.000000000000000000, 1.000000000000000000 ) ) ;
#2824 = CARTESIAN_POINT ( 'NONE',  ( 0.7871730179869745880, 0.2548056305271102495, -0.2803186531705669227 ) ) ;
#2825 = CARTESIAN_POINT ( 'NONE',  ( -0.3263749705684267921, -0.1890319631540330891, 0.1992125984251968684 ) ) ;
#2826 = VECTOR ( 'NONE', #2224, 39.37007874015748143 ) ;
#2827 = ( BOUNDED_CURVE ( )  B_SPLINE_CURVE ( 2, ( #16964, #14869, #4109 ),
 .UNSPECIFIED., .F., .T. ) 
 B_SPLINE_CURVE_WITH_KNOTS ( ( 3, 3 ),
 ( 0.000000000000000000, 0.5842180690389568998 ),
 .UNSPECIFIED. ) 
 CURVE ( )  GEOMETRIC_REPRESENTATION_ITEM ( )  RATIONAL_B_SPLINE_CURVE ( ( 1.000000000000000000, 1.154700538379249908, 1.000000000000000000 ) ) 
 REPRESENTATION_ITEM ( '' )  ) ;
#2828 = AXIS2_PLACEMENT_3D ( 'NONE', #13039, #9067, #26302 ) ;
#2829 = DIRECTION ( 'NONE',  ( 0.9848077530122081313, 0.1736481776669299981, -0.000000000000000000 ) ) ;
#2830 = CARTESIAN_POINT ( 'NONE',  ( 0.09842519685039370636, 0.2165354330708661457, -3.272637795275590733 ) ) ;
#2831 = EDGE_LOOP ( 'NONE', ( #11493, #11739, #18792, #21781 ) ) ;
#2832 = CARTESIAN_POINT ( 'NONE',  ( -0.2521176338356572177, -0.2211428102655754180, 1.973425196850393970 ) ) ;
#2833 = CARTESIAN_POINT ( 'NONE',  ( -0.1707210962531915677, -0.4707890492249701131, 0.2574803149606298969 ) ) ;
#2834 = CARTESIAN_POINT ( 'NONE',  ( -0.4423390553432768879, -0.2180862235769457091, -1.550196850393700920 ) ) ;
#2835 = CARTESIAN_POINT ( 'NONE',  ( 0.000000000000000000, 0.07874015746264864668, 0.5905511811200284678 ) ) ;
#2836 = CARTESIAN_POINT ( 'NONE',  ( 0.06001958459476169905, -0.4555658499976140696, -1.928289503579150077 ) ) ;
#2837 = AXIS2_PLACEMENT_3D ( 'NONE', #4234, #8058, #16514 ) ;
#2838 = CARTESIAN_POINT ( 'NONE',  ( 0.1429116519061275903, 0.5335524835332325910, 0.9202755905511811330 ) ) ;
#2839 = CARTESIAN_POINT ( 'NONE',  ( -0.05118110236220472370, 0.8267716535433071723, 0.000000000000000000 ) ) ;
#2840 = AXIS2_PLACEMENT_3D ( 'NONE', #15686, #7071, #20057 ) ;
#2841 = CARTESIAN_POINT ( 'NONE',  ( -0.3584231247409862542, 0.000000000000000000, -0.05511811023622047168 ) ) ;
#2842 = DIRECTION ( 'NONE',  ( -1.000000000000000000, 0.000000000000000000, 0.000000000000000000 ) ) ;
#2843 = CARTESIAN_POINT ( 'NONE',  ( -0.4763861460130329739, 0.1275996891957754675, -1.569881889763779625 ) ) ;
#2844 = CARTESIAN_POINT ( 'NONE',  ( -0.6370261810203012853, -0.06929385342672342296, 0.2344319926069744209 ) ) ;
#2845 = LINE ( 'NONE', #11483, #16951 ) ;
#2846 = DIRECTION ( 'NONE',  ( 0.2588190448135643806, 0.000000000000000000, 0.9659258263664939337 ) ) ;
#2847 = CARTESIAN_POINT ( 'NONE',  ( -0.5699748819080105999, -0.3282885190149778531, 0.2081850588304353933 ) ) ;
#2848 = EDGE_CURVE ( 'NONE', #16503, #16500, #23255, .T. ) ;
#2849 = CLOSED_SHELL ( 'NONE', ( #19233, #19425, #7267, #3992, #27872, #3766, #16838, #549, #518, #21735, #15372, #5394, #24391, #24830, #4706, #6449, #19552, #6236, #23916, #4940, #4260, #15149, #16729, #21569, #22767, #11069, #663, #19835, #22092, #3616, #10112, #7090, #6231, #6239, #23934, #408, #27024, #12980, #20774, #11670, #18690, #18113, #24949, #13433, #22326, #1019, #1623, #1919, #10233, #25707, #18777, #12122, #10296, #2236, #13299, #4620 ) ) ;
#2850 = PLANE ( 'NONE',  #16081 ) ;
#2851 = DIRECTION ( 'NONE',  ( 0.000000000000000000, 0.000000000000000000, -1.000000000000000000 ) ) ;
#2852 = ORIENTED_EDGE ( 'NONE', *, *, #10985, .F. ) ;
#2853 = DIRECTION ( 'NONE',  ( 1.000000000000000000, 7.017815000000030939E-18, 0.000000000000000000 ) ) ;
#2854 = VERTEX_POINT ( 'NONE', #11783 ) ;
#2855 = AXIS2_PLACEMENT_3D ( 'NONE', #1583, #18370, #12041 ) ;
#2856 = CARTESIAN_POINT ( 'NONE',  ( 0.4069519308877023178, -0.2006393256663573099, -1.934055118110236338 ) ) ;
#2857 = CARTESIAN_POINT ( 'NONE',  ( 0.4216927985368217335, -0.2427835582310488571, 0.09284957166208239465 ) ) ;
#2858 = CARTESIAN_POINT ( 'NONE',  ( 0.5699748819079695217, -0.3282885190149665844, 0.2081850588305529104 ) ) ;
#2859 = CYLINDRICAL_SURFACE ( 'NONE', #19118, 0.8267716535433071723 ) ;
#2860 = VECTOR ( 'NONE', #11180, 39.37007874015748143 ) ;
#2861 = DIRECTION ( 'NONE',  ( 0.000000000000000000, -1.000000000000000000, 0.000000000000000000 ) ) ;
#2862 = CARTESIAN_POINT ( 'NONE',  ( -0.2952755905264887182, 3.616083068046089993E-17, 2.090519358671640647E-11 ) ) ;
#2863 = DIRECTION ( 'NONE',  ( 0.000000000000000000, 1.000000000000000000, 0.000000000000000000 ) ) ;
#2864 = CARTESIAN_POINT ( 'NONE',  ( 0.000000000000000000, 0.000000000000000000, 0.2755905511811023723 ) ) ;
#2865 = DIRECTION ( 'NONE',  ( 1.000000000000000000, 0.000000000000000000, 0.000000000000000000 ) ) ;
#2866 = CARTESIAN_POINT ( 'NONE',  ( -0.3740848232703756771, 0.04928467685643712209, -3.100567304031759175 ) ) ;
#2867 = DIRECTION ( 'NONE',  ( 0.000000000000000000, -7.180547322999995702E-06, -0.9999999999742197332 ) ) ;
#2868 = DIRECTION ( 'NONE',  ( 0.000000000000000000, 0.000000000000000000, -1.000000000000000000 ) ) ;
#2869 = AXIS2_PLACEMENT_3D ( 'NONE', #18516, #16415, #14173 ) ;
#2870 = ORIENTED_EDGE ( 'NONE', *, *, #10426, .F. ) ;
#2871 = EDGE_CURVE ( 'NONE', #20420, #3990, #24254, .T. ) ;
#2872 = CARTESIAN_POINT ( 'NONE',  ( -0.4300129863948120579, -0.2478439864030019535, -1.569881889763780070 ) ) ;
#2873 = PRODUCT_CONTEXT ( 'NONE', #22595, 'mechanical' ) ;
#2874 = AXIS2_PLACEMENT_3D ( 'NONE', #10156, #27408, #8066 ) ;
#2875 = ORIENTED_EDGE ( 'NONE', *, *, #4475, .T. ) ;
#2876 = B_SPLINE_CURVE_WITH_KNOTS ( 'NONE', 3,
 ( #15346, #23939, #8947, #6846, #15472, #15608 ),
 .UNSPECIFIED., .F., .F.,
 ( 4, 2, 4 ),
 ( 0.002631077521236949331, 0.003072896085239190580, 0.003514714649241431829 ),
 .UNSPECIFIED. ) ;
#2877 = EDGE_CURVE ( 'NONE', #2281, #2854, #18362, .T. ) ;
#2878 = AXIS2_PLACEMENT_3D ( 'NONE', #378, #3646, #18474 ) ;
#2879 = ORIENTED_EDGE ( 'NONE', *, *, #24423, .T. ) ;
#2880 = FACE_OUTER_BOUND ( 'NONE', #3212, .T. ) ;
#2881 = CARTESIAN_POINT ( 'NONE',  ( -0.4157391792961063204, 0.3323952789219086768, 0.3401574803149606252 ) ) ;
#2882 = CARTESIAN_POINT ( 'NONE',  ( 0.03349795313264332386, 0.5118110236220472231, 1.747047244094488194 ) ) ;
#2883 = CARTESIAN_POINT ( 'NONE',  ( -0.06699507805371239522, -0.5085118447801502128, 1.747047244094488194 ) ) ;
#2884 = ( NAMED_UNIT ( * ) SI_UNIT ( $, .STERADIAN. ) SOLID_ANGLE_UNIT ( ) ) ;
#2885 = VERTEX_POINT ( 'NONE', #24357 ) ;
#2886 = CARTESIAN_POINT ( 'NONE',  ( -0.04877294052296160531, 0.3702005978258477437, -3.115157480314960647 ) ) ;
#2887 = ORIENTED_EDGE ( 'NONE', *, *, #20186, .T. ) ;
#2888 = CARTESIAN_POINT ( 'NONE',  ( 0.7874015748031496509, 0.2724655384146937864, -0.2020072023942773021 ) ) ;
#2889 = DIRECTION ( 'NONE',  ( 0.000000000000000000, 0.000000000000000000, 1.000000000000000000 ) ) ;
#2890 = AXIS2_PLACEMENT_3D ( 'NONE', #2515, #2652, #11278 ) ;
#2891 = ORIENTED_EDGE ( 'NONE', *, *, #7871, .F. ) ;
#2892 = ORIENTED_EDGE ( 'NONE', *, *, #1435, .F. ) ;
#2893 = CARTESIAN_POINT ( 'NONE',  ( 0.1516263115863346334, -0.4909405214979283838, -0.05579628926458622684 ) ) ;
#2894 = CARTESIAN_POINT ( 'NONE',  ( -0.1599629598573265865, -0.4411872753632007926, 0.1992125984251968684 ) ) ;
#2895 = ORIENTED_EDGE ( 'NONE', *, *, #13667, .T. ) ;
#2896 = B_SPLINE_CURVE_WITH_KNOTS ( 'NONE', 3,
 ( #11826, #20446, #3333, #16216, #20160, #17882 ),
 .UNSPECIFIED., .F., .F.,
 ( 4, 2, 4 ),
 ( 0.3000437156586439613, 0.3015484798814569989, 0.3030532441042709801 ),
 .UNSPECIFIED. ) ;
#2897 = CARTESIAN_POINT ( 'NONE',  ( 0.4303822302053771365, 0.1152775731717053109, -1.934055118110236338 ) ) ;
#2898 = ORIENTED_EDGE ( 'NONE', *, *, #24019, .F. ) ;
#2899 = DIRECTION ( 'NONE',  ( 0.000000000000000000, 0.000000000000000000, 1.000000000000000000 ) ) ;
#2900 = CARTESIAN_POINT ( 'NONE',  ( 0.2303471512294322787, -0.4798602677570401598, 0.3401574803149606252 ) ) ;
#2901 = AXIS2_PLACEMENT_3D ( 'NONE', #27696, #24860, #14143 ) ;
#2902 = EDGE_CURVE ( 'NONE', #16455, #17891, #6228, .T. ) ;
#2903 = DIRECTION ( 'NONE',  ( 0.000000000000000000, 0.000000000000000000, 1.000000000000000000 ) ) ;
#2904 = CONICAL_SURFACE ( 'NONE', #12415, 1.112204724409448842, 0.7853981625000011624 ) ;
#2905 = DIRECTION ( 'NONE',  ( 0.000000000000000000, 0.000000000000000000, -1.000000000000000000 ) ) ;
#2906 = FACE_OUTER_BOUND ( 'NONE', #24076, .T. ) ;
#2907 = DIRECTION ( 'NONE',  ( 0.000000000000000000, 0.000000000000000000, -1.000000000000000000 ) ) ;
#2908 = CARTESIAN_POINT ( 'NONE',  ( -0.04956879728060034629, 0.2165354330708661734, -3.186635197996628310 ) ) ;
#2909 = EDGE_CURVE ( 'NONE', #4618, #17370, #9814, .T. ) ;
#2910 = CARTESIAN_POINT ( 'NONE',  ( -0.3259357382551450466, -0.08759279594700321303, 1.973425196850394192 ) ) ;
#2911 = EDGE_CURVE ( 'NONE', #2567, #858, #13621, .T. ) ;
#2912 = ADVANCED_FACE ( 'NONE', ( #18261 ), #1262, .T. ) ;
#2913 = AXIS2_PLACEMENT_3D ( 'NONE', #14096, #26953, #965 ) ;
#2914 = DIRECTION ( 'NONE',  ( 0.7071067818211439482, 8.659560570126498371E-17, -0.7071067805519510863 ) ) ;
#2915 = DIRECTION ( 'NONE',  ( 0.000000000000000000, 1.000000000000000000, 0.000000000000000000 ) ) ;
#2916 = DIRECTION ( 'NONE',  ( 0.000000000000000000, 0.000000000000000000, -1.000000000000000000 ) ) ;
#2917 = EDGE_CURVE ( 'NONE', #23029, #19454, #20648, .T. ) ;
#2918 = CARTESIAN_POINT ( 'NONE',  ( 0.1599629598573263645, -0.4411872753632007926, 0.1992125984251968684 ) ) ;
#2919 = CARTESIAN_POINT ( 'NONE',  ( -0.5144970376935736889, 0.1378076643338841389, 1.747047244094488194 ) ) ;
#2920 = VERTEX_POINT ( 'NONE', #21971 ) ;
#2921 = CARTESIAN_POINT ( 'NONE',  ( 0.4302903874081785984, -0.2491168502844573474, 0.1140743250896437688 ) ) ;
#2922 = VERTEX_POINT ( 'NONE', #11640 ) ;
#2923 = CIRCLE ( 'NONE', #4729, 0.6614173228346456046 ) ;
#2924 = CARTESIAN_POINT ( 'NONE',  ( 0.3339160553493877859, 5.862181872598426086E-06, -1.869015748010449007 ) ) ;
#2925 = ( NAMED_UNIT ( * ) PLANE_ANGLE_UNIT ( ) SI_UNIT ( $, .RADIAN. ) ) ;
#2926 = EDGE_LOOP ( 'NONE', ( #26692, #19413, #18428, #2665 ) ) ;
#2927 = DIRECTION ( 'NONE',  ( -0.000000000000000000, -1.000000000000000000, -0.000000000000000000 ) ) ;
#2928 = ORIENTED_EDGE ( 'NONE', *, *, #27409, .F. ) ;
#2929 = CARTESIAN_POINT ( 'NONE',  ( -0.3252100150720461658, 0.3707612262532960501, -1.569881889763779625 ) ) ;
#2930 = DIRECTION ( 'NONE',  ( 0.000000000000000000, 1.000000000000000000, 0.000000000000000000 ) ) ;
#2931 = ORIENTED_EDGE ( 'NONE', *, *, #15459, .F. ) ;
#2932 = CARTESIAN_POINT ( 'NONE',  ( -0.3642352168757849173, -0.4152525734086955356, 0.9399606299212598381 ) ) ;
#2933 = DIMENSIONAL_EXPONENTS ( 1.000000000000000000, 0.000000000000000000, 0.000000000000000000, 0.000000000000000000, 0.000000000000000000, 0.000000000000000000, 0.000000000000000000 ) ;
#2934 = ORIENTED_EDGE ( 'NONE', *, *, #7754, .F. ) ;
#2935 = CIRCLE ( 'NONE', #13318, 0.4803149606299212393 ) ;
#2936 = DIRECTION ( 'NONE',  ( -0.9848077530122082424, -0.1736481776669300259, 0.000000000000000000 ) ) ;
#2937 = DIRECTION ( 'NONE',  ( 0.000000000000000000, 0.000000000000000000, 1.000000000000000000 ) ) ;
#2938 = DIRECTION ( 'NONE',  ( 0.000000000000000000, 0.000000000000000000, 1.000000000000000000 ) ) ;
#2939 = CARTESIAN_POINT ( 'NONE',  ( -0.0005789383928838939082, 0.4762008496974535765, 0.2330651857776422364 ) ) ;
#2940 = FACE_OUTER_BOUND ( 'NONE', #4320, .T. ) ;
#2941 = DIRECTION ( 'NONE',  ( 0.000000000000000000, -1.000000000000000000, 0.000000000000000000 ) ) ;
#2942 = ADVANCED_FACE ( 'NONE', ( #13763 ), #19849, .T. ) ;
#2943 = CYLINDRICAL_SURFACE ( 'NONE', #8673, 0.5007874015748031704 ) ;
#2944 = CARTESIAN_POINT ( 'NONE',  ( 0.01453548245982153216, 0.08252923752360777354, -0.4702630791244896136 ) ) ;
#2945 = FACE_OUTER_BOUND ( 'NONE', #13500, .T. ) ;
#2946 = TOROIDAL_SURFACE ( 'NONE', #18286, 0.6102362204724409711, 0.1299212598425196763 ) ;
#2947 = EDGE_CURVE ( 'NONE', #24281, #22748, #24233, .T. ) ;
#2948 = DIRECTION ( 'NONE',  ( 0.000000000000000000, 1.000000000000000000, 0.000000000000000000 ) ) ;
#2949 = CARTESIAN_POINT ( 'NONE',  ( -0.3209354104562381349, 0.3834063931592568419, 0.1496602734580050054 ) ) ;
#2950 = CARTESIAN_POINT ( 'NONE',  ( 0.8558003517949211991, 0.6468501409757874132, 2.027559055118110187 ) ) ;
#2951 = AXIS2_PLACEMENT_3D ( 'NONE', #17165, #15609, #13060 ) ;
#2952 = CARTESIAN_POINT ( 'NONE',  ( 0.4216473063928389275, -0.2427620699807058191, 0.1075369453624760163 ) ) ;
#2953 = CARTESIAN_POINT ( 'NONE',  ( 0.3339160553493882300, 0.000000000000000000, -1.052618110236220428 ) ) ;
#2954 = CYLINDRICAL_SURFACE ( 'NONE', #14208, 0.1771653543307086798 ) ;
#2955 = CYLINDRICAL_SURFACE ( 'NONE', #4382, 0.6299212598425196763 ) ;
#2956 = ADVANCED_FACE ( 'NONE', ( #9507, #11506 ), #18107, .T. ) ;
#2957 = ORIENTED_EDGE ( 'NONE', *, *, #27118, .T. ) ;
#2958 = CARTESIAN_POINT ( 'NONE',  ( -0.4895985792973480133, 0.000000000000000000, 0.000000000000000000 ) ) ;
#2959 = CIRCLE ( 'NONE', #13813, 0.6881889763779527325 ) ;
#2960 = LINE ( 'NONE', #20072, #13900 ) ;
#2961 = EDGE_LOOP ( 'NONE', ( #5163, #7139, #19666, #17295 ) ) ;
#2962 = DIRECTION ( 'NONE',  ( -1.000000000000000000, 0.000000000000000000, 0.000000000000000000 ) ) ;
#2963 = ORIENTED_EDGE ( 'NONE', *, *, #26481, .F. ) ;
#2964 = AXIS2_PLACEMENT_3D ( 'NONE', #20804, #14767, #7960 ) ;
#2965 = CARTESIAN_POINT ( 'NONE',  ( 0.7430739993161732393, 0.6166684212952147082, -0.09296748371178542580 ) ) ;
#2966 = EDGE_CURVE ( 'NONE', #10287, #1952, #26468, .T. ) ;
#2967 = DIRECTION ( 'NONE',  ( 0.000000000000000000, -1.000000000000000000, 0.000000000000000000 ) ) ;
#2968 = ORIENTED_EDGE ( 'NONE', *, *, #21663, .F. ) ;
#2969 = EDGE_CURVE ( 'NONE', #12210, #21566, #5764, .T. ) ;
#2970 = EDGE_LOOP ( 'NONE', ( #22132, #13262 ) ) ;
#2971 = CARTESIAN_POINT ( 'NONE',  ( -0.2521176338356575508, 0.2211428102655751127, 1.973425196850393970 ) ) ;
#2972 = CARTESIAN_POINT ( 'NONE',  ( 0.3912931228432192099, -0.3001918266902123267, -1.550196850393700920 ) ) ;
#2973 = EDGE_CURVE ( 'NONE', #18986, #1498, #26337, .T. ) ;
#2974 = DIRECTION ( 'NONE',  ( 1.000000000000000000, 0.000000000000000000, 0.000000000000000000 ) ) ;
#2975 = CARTESIAN_POINT ( 'NONE',  ( 0.06894484415506239861, -0.05111597790242464190, -0.4724409448818898127 ) ) ;
#2976 = CARTESIAN_POINT ( 'NONE',  ( 0.3642352168757554964, -0.4152525734086275899, 0.9202755905511811330 ) ) ;
#2977 = DIRECTION ( 'NONE',  ( 0.6234898018587335944, 0.7818314824680296926, 0.000000000000000000 ) ) ;
#2978 = AXIS2_PLACEMENT_3D ( 'NONE', #22942, #16569, #3559 ) ;
#2979 = FACE_OUTER_BOUND ( 'NONE', #26175, .T. ) ;
#2980 = DIRECTION ( 'NONE',  ( 0.000000000000000000, 0.000000000000000000, 1.000000000000000000 ) ) ;
#2981 = CARTESIAN_POINT ( 'NONE',  ( -0.3001918266902143251, 0.3912931228432222075, -1.569881889763779625 ) ) ;
#2982 = AXIS2_PLACEMENT_3D ( 'NONE', #6922, #558, #9155 ) ;
#2983 = LINE ( 'NONE', #6775, #17603 ) ;
#2984 = CARTESIAN_POINT ( 'NONE',  ( 0.3667188884249754643, 0.2611681335937625636, 0.2162202218317502145 ) ) ;
#2985 = CARTESIAN_POINT ( 'NONE',  ( 0.0005696707463077370576, 0.4606295689977898400, 0.1771653543307089018 ) ) ;
#2986 = CARTESIAN_POINT ( 'NONE',  ( -0.5491102354215389170, -0.3162573801172571808, 0.2481708550950527947 ) ) ;
#2987 = EDGE_CURVE ( 'NONE', #5913, #9216, #24812, .T. ) ;
#2988 = DIRECTION ( 'NONE',  ( 1.000000000000000000, 0.000000000000000000, 0.000000000000000000 ) ) ;
#2989 = DIRECTION ( 'NONE',  ( 0.000000000000000000, 1.000000000000000000, 0.000000000000000000 ) ) ;
#2990 = ORIENTED_EDGE ( 'NONE', *, *, #13862, .F. ) ;
#2991 = CARTESIAN_POINT ( 'NONE',  ( 0.1775220790477149424, 0.3075317527317797395, 1.953740157480315043 ) ) ;
#2992 = ORIENTED_EDGE ( 'NONE', *, *, #6972, .T. ) ;
#2993 = ( BOUNDED_CURVE ( )  B_SPLINE_CURVE ( 2, ( #2719, #11082, #17834 ),
 .UNSPECIFIED., .F., .T. ) 
 B_SPLINE_CURVE_WITH_KNOTS ( ( 3, 3 ),
 ( 0.000000000000000000, 0.2336872276155829986 ),
 .UNSPECIFIED. ) 
 CURVE ( )  GEOMETRIC_REPRESENTATION_ITEM ( )  RATIONAL_B_SPLINE_CURVE ( ( 1.000000000000000000, 1.154700538379249908, 1.000000000000000000 ) ) 
 REPRESENTATION_ITEM ( '' )  ) ;
#2994 = CARTESIAN_POINT ( 'NONE',  ( -0.2761764805255463306, -0.3599896729929341621, -1.934055118110236338 ) ) ;
#2995 = CARTESIAN_POINT ( 'NONE',  ( -0.3726024258163779246, 0.02438677169354841121, -3.115157480314960647 ) ) ;
#2996 = CARTESIAN_POINT ( 'NONE',  ( 0.4333114377122374572, -0.2494818589555374000, 0.1496602734576668314 ) ) ;
#2997 = CARTESIAN_POINT ( 'NONE',  ( -0.06894484415077309358, 0.05111597790490104293, -0.4724409448818898127 ) ) ;
#2998 = DIRECTION ( 'NONE',  ( 0.000000000000000000, 0.000000000000000000, 1.000000000000000000 ) ) ;
#2999 = ( GEOMETRIC_REPRESENTATION_CONTEXT ( 3 ) GLOBAL_UNCERTAINTY_ASSIGNED_CONTEXT ( ( #24565 ) ) GLOBAL_UNIT_ASSIGNED_CONTEXT ( ( #17236, #18926, #25289 ) ) REPRESENTATION_CONTEXT ( 'NONE', 'WORKASPACE' ) ) ;
#3000 = DIRECTION ( 'NONE',  ( -0.000000000000000000, -1.000000000000000000, -0.000000000000000000 ) ) ;
#3001 = DIRECTION ( 'NONE',  ( 0.000000000000000000, 0.000000000000000000, -1.000000000000000000 ) ) ;
#3002 = CARTESIAN_POINT ( 'NONE',  ( 0.003937007874015826907, -4.393043307086613241E-18, 0.000000000000000000 ) ) ;
#3003 = CARTESIAN_POINT ( 'NONE',  ( 0.2993674444872273521, 0.2296683860596781812, -3.100567304031764060 ) ) ;
#3004 = CARTESIAN_POINT ( 'NONE',  ( 0.000000000000000000, 0.000000000000000000, 0.07637795275590551769 ) ) ;
#3005 = EDGE_CURVE ( 'NONE', #14102, #6801, #12966, .T. ) ;
#3006 = ORIENTED_EDGE ( 'NONE', *, *, #5390, .T. ) ;
#3007 = CARTESIAN_POINT ( 'NONE',  ( -0.4921259842519686845, -0.06441914069860964209, -1.569881889763780070 ) ) ;
#3008 = EDGE_CURVE ( 'NONE', #23052, #25295, #24687, .T. ) ;
#3009 = APPLICATION_PROTOCOL_DEFINITION ( 'draft international standard', 'automotive_design', 1998, #1154 ) ;
#3010 = CARTESIAN_POINT ( 'NONE',  ( -0.7246715730664488042, 0.1595564285404119931, -0.2516711161248811335 ) ) ;
#3011 = ORIENTED_EDGE ( 'NONE', *, *, #578, .F. ) ;
#3012 = AXIS2_PLACEMENT_3D ( 'NONE', #14621, #12471, #21084 ) ;
#3013 = STYLED_ITEM ( 'NONE', ( #6589 ), #2707 ) ;
#3014 = CARTESIAN_POINT ( 'NONE',  ( -0.3503688343903059166, -1.161116239014858387, -0.4867237306978748346 ) ) ;
#3015 = DIRECTION ( 'NONE',  ( 0.2036417511401769631, -0.9790454724845838452, 1.198984999999999849E-16 ) ) ;
#3016 = CARTESIAN_POINT ( 'NONE',  ( 0.1327036767659575123, -0.4954415918530866714, 1.766732283464566899 ) ) ;
#3017 = ORIENTED_EDGE ( 'NONE', *, *, #6004, .T. ) ;
#3018 = ( LENGTH_UNIT ( ) NAMED_UNIT ( * ) SI_UNIT ( $, .METRE. ) ) ;
#3019 = B_SPLINE_CURVE_WITH_KNOTS ( 'NONE', 3,
 ( #8186, #25271, #26975, #1130 ),
 .UNSPECIFIED., .F., .F.,
 ( 4, 4 ),
 ( 0.9893485554301200136, 0.9909948584944189287 ),
 .UNSPECIFIED. ) ;
#3020 = CIRCLE ( 'NONE', #18825, 0.4921259842519685179 ) ;
#3021 = CARTESIAN_POINT ( 'NONE',  ( 0.3233561589689049054, 0.1867299569291689110, -3.115157480314960647 ) ) ;
#3022 = MANIFOLD_SOLID_BREP ( 'Shaft Seal 20x35x7', #25894 ) ;
#3023 = ORIENTED_EDGE ( 'NONE', *, *, #2564, .T. ) ;
#3024 = CARTESIAN_POINT ( 'NONE',  ( -0.03937007874015747977, 0.000000000000000000, 0.000000000000000000 ) ) ;
#3025 = ORIENTED_EDGE ( 'NONE', *, *, #10718, .F. ) ;
#3026 = ORIENTED_EDGE ( 'NONE', *, *, #57, .T. ) ;
#3028 = ADVANCED_FACE ( 'NONE', ( #7978 ), #3039, .F. ) ;
#3027 = VERTEX_POINT ( 'NONE', #12489 ) ;
#3029 = EDGE_LOOP ( 'NONE', ( #11928, #9052, #17562, #5731, #24652 ) ) ;
#3030 = CARTESIAN_POINT ( 'NONE',  ( 0.1291602287245497971, -0.3543605079199910191, 0.1992150590373740204 ) ) ;
#3031 = CARTESIAN_POINT ( 'NONE',  ( -0.05118110236220472370, 0.000000000000000000, 0.000000000000000000 ) ) ;
#3032 = ORIENTED_EDGE ( 'NONE', *, *, #24525, .T. ) ;
#3033 = CARTESIAN_POINT ( 'NONE',  ( 0.1152775731716972618, -0.4303822302053990634, -1.934055118110236338 ) ) ;
#3034 = CARTESIAN_POINT ( 'NONE',  ( -0.3223547283257516272, 0.3832433309296771617, 0.09685039370078740717 ) ) ;
#3035 = DIRECTION ( 'NONE',  ( 1.000000000000000000, 0.000000000000000000, 0.000000000000000000 ) ) ;
#3036 = AXIS2_PLACEMENT_3D ( 'NONE', #19500, #25728, #6375 ) ;
#3037 = CARTESIAN_POINT ( 'NONE',  ( 0.3843128886798082844, 0.2238742596014886010, 0.2362204724409449064 ) ) ;
#3038 = FACE_OUTER_BOUND ( 'NONE', #25601, .T. ) ;
#3039 = CONICAL_SURFACE ( 'NONE', #21114, 0.04546065111729338803, 1.047197549999998811 ) ;
#3040 = CARTESIAN_POINT ( 'NONE',  ( 0.3346456692913385988, 2.049113738730807321E-17, 1.973425196850393970 ) ) ;
#3041 = DIRECTION ( 'NONE',  ( 0.000000000000000000, 1.000000000000000000, 0.000000000000000000 ) ) ;
#3042 = PRODUCT_DEFINITION_SHAPE ( 'NONE', 'NONE',  #27909 ) ;
#3043 = DIRECTION ( 'NONE',  ( -0.000000000000000000, -1.000000000000000000, -0.000000000000000000 ) ) ;
#3044 = FACE_OUTER_BOUND ( 'NONE', #26076, .T. ) ;
#3045 = SURFACE_SIDE_STYLE ('',( #5177 ) ) ;
#3046 = CARTESIAN_POINT ( 'NONE',  ( 0.1141709026133643362, 0.3362336590883639453, 1.953740157480315043 ) ) ;
#3047 = B_SPLINE_CURVE_WITH_KNOTS ( 'NONE', 3,
 ( #15958, #12272, #25128, #24558, #9578, #10015 ),
 .UNSPECIFIED., .F., .F.,
 ( 4, 2, 4 ),
 ( 0.7157687286427140139, 0.7172350147555670574, 0.7187013008684189908 ),
 .UNSPECIFIED. ) ;
#3048 = FACE_OUTER_BOUND ( 'NONE', #23019, .T. ) ;
#3049 = CARTESIAN_POINT ( 'NONE',  ( -0.3338887748335570005, -1.256685249340607546, -0.7575795143361759854 ) ) ;
#3050 = DIRECTION ( 'NONE',  ( 1.000000000000000000, 0.000000000000000000, 0.000000000000000000 ) ) ;
#3051 = CARTESIAN_POINT ( 'NONE',  ( 0.000000000000000000, 0.000000000000000000, 0.4488188976377953110 ) ) ;
#3052 = CARTESIAN_POINT ( 'NONE',  ( -0.5144970376935739109, -0.1378076643338908835, 1.747047244094488194 ) ) ;
#3053 = CARTESIAN_POINT ( 'NONE',  ( -0.1327036767659680594, 0.4954415918530845619, 1.766732283464566899 ) ) ;
#3054 = TOROIDAL_SURFACE ( 'NONE', #18860, 0.4232283464566928832, 0.07677165354330708902 ) ;
#3055 = AXIS2_PLACEMENT_3D ( 'NONE', #14460, #3688, #12316 ) ;
#3056 = FACE_OUTER_BOUND ( 'NONE', #16842, .T. ) ;
#3057 = ORIENTED_EDGE ( 'NONE', *, *, #24084, .T. ) ;
#3058 = MECHANICAL_DESIGN_GEOMETRIC_PRESENTATION_REPRESENTATION (  '', ( #18409 ), #19323 ) ;
#3059 = ( CONVERSION_BASED_UNIT ( 'INCH', #5779 ) LENGTH_UNIT ( ) NAMED_UNIT ( #6927 ) ) ;
#3060 = ORIENTED_EDGE ( 'NONE', *, *, #11134, .T. ) ;
#3061 = DIRECTION ( 'NONE',  ( 0.000000000000000000, 1.000000000000000000, 0.000000000000000000 ) ) ;
#3062 = EDGE_CURVE ( 'NONE', #17898, #14958, #14383, .T. ) ;
#3063 = ORIENTED_EDGE ( 'NONE', *, *, #15128, .T. ) ;
#3064 = CARTESIAN_POINT ( 'NONE',  ( 0.4270824798167637826, -0.2466292688015195855, -1.569881889763779625 ) ) ;
#3065 = AXIS2_PLACEMENT_3D ( 'NONE', #13857, #11454, #876 ) ;
#3066 = ORIENTED_EDGE ( 'NONE', *, *, #5730, .T. ) ;
#3067 = CARTESIAN_POINT ( 'NONE',  ( -0.5476281405333571772, -0.07214854559198842499, 0.9399606299212598381 ) ) ;
#3068 = EDGE_LOOP ( 'NONE', ( #12674, #2875, #25773, #20146 ) ) ;
#3069 = ADVANCED_FACE ( 'NONE', ( #6279 ), #14838, .F. ) ;
#3070 = ORIENTED_EDGE ( 'NONE', *, *, #9051, .T. ) ;
#3071 = FACE_BOUND ( 'NONE', #10220, .T. ) ;
#3072 = DIRECTION ( 'NONE',  ( -0.9790454724845842893, -0.1018208755700880375, 0.1763589297585410332 ) ) ;
#3073 = CONTEXT_DEPENDENT_SHAPE_REPRESENTATION ( #26065, #16160 ) ;
#3074 = EDGE_CURVE ( 'NONE', #14891, #4135, #23792, .T. ) ;
#3075 = DIRECTION ( 'NONE',  ( 0.000000000000000000, -1.000000000000000000, 0.000000000000000000 ) ) ;
#3076 = MANIFOLD_SOLID_BREP ( 'Front Bearing Cover', #11437 ) ;
#3077 = DIRECTION ( 'NONE',  ( 0.000000000000000000, 0.000000000000000000, 1.000000000000000000 ) ) ;
#3078 = DIRECTION ( 'NONE',  ( -1.000000000000000000, 0.000000000000000000, 0.000000000000000000 ) ) ;
#3079 = FACE_OUTER_BOUND ( 'NONE', #14199, .T. ) ;
#3080 = AXIS2_PLACEMENT_3D ( 'NONE', #20906, #1550, #16814 ) ;
#3081 = CARTESIAN_POINT ( 'NONE',  ( -0.4157391792961063204, 0.3323952789219086768, 0.3401574803149606252 ) ) ;
#3082 = CARTESIAN_POINT ( 'NONE',  ( -0.4222761783109335032, 0.5043089796502874256, 0.2081850588267502022 ) ) ;
#3083 = AXIS2_PLACEMENT_3D ( 'NONE', #23793, #9069, #4438 ) ;
#3084 = CARTESIAN_POINT ( 'NONE',  ( 0.3239425792934414461, -0.08676778863010961573, 1.953740157480315043 ) ) ;
#3085 = UNCERTAINTY_MEASURE_WITH_UNIT (LENGTH_MEASURE( 1.000000000000000082E-05 ), #4516, 'distance_accuracy_value', 'NONE') ;
#3086 = ORIENTED_EDGE ( 'NONE', *, *, #17207, .F. ) ;
#3087 = DIRECTION ( 'NONE',  ( 0.5000000010362839475, -1.060575237992202059E-16, -0.8660254031861397417 ) ) ;
#3088 = CARTESIAN_POINT ( 'NONE',  ( 0.0007595033562148819414, 0.6881885572739390167, 0.1322834645669291320 ) ) ;
#3089 = DIRECTION ( 'NONE',  ( -1.000000000000000000, 0.000000000000000000, 0.000000000000000000 ) ) ;
#3090 = CARTESIAN_POINT ( 'NONE',  ( -0.1286734528930088550, -0.3545375539099149265, 0.07637630750536809898 ) ) ;
#3091 = DIRECTION ( 'NONE',  ( 0.000000000000000000, 1.000000000000000000, 0.000000000000000000 ) ) ;
#3092 = DIRECTION ( 'NONE',  ( 0.000000000000000000, 1.000000000000000000, 0.000000000000000000 ) ) ;
#3093 = B_SPLINE_CURVE_WITH_KNOTS ( 'NONE', 3,
 ( #702, #22308, #2939, #14710, #14845, #8185 ),
 .UNSPECIFIED., .F., .F.,
 ( 4, 2, 4 ),
 ( 0.000000000000000000, 0.2500000000000000000, 0.5000000000000000000 ),
 .UNSPECIFIED. ) ;
#3094 = EDGE_CURVE ( 'NONE', #10030, #4351, #19419, .T. ) ;
#3095 = LENGTH_MEASURE_WITH_UNIT ( LENGTH_MEASURE( 0.02539999999999999897 ), #22747 ) ;
#3096 = ORIENTED_EDGE ( 'NONE', *, *, #1444, .F. ) ;
#3097 = ADVANCED_FACE ( 'NONE', ( #2906 ), #20667, .T. ) ;
#3098 = EDGE_CURVE ( 'NONE', #18478, #18898, #7298, .T. ) ;
#3099 = AXIS2_PLACEMENT_3D ( 'NONE', #25907, #6556, #5249 ) ;
#3100 = CYLINDRICAL_SURFACE ( 'NONE', #26407, 0.6299212598425196763 ) ;
#3101 = ( REPRESENTATION_RELATIONSHIP ('NONE','NONE', #12434, #16232 ) REPRESENTATION_RELATIONSHIP_WITH_TRANSFORMATION ( #14119 )SHAPE_REPRESENTATION_RELATIONSHIP( ) ) ;
#3102 = CARTESIAN_POINT ( 'NONE',  ( 0.000000000000000000, 0.000000000000000000, 0.2755905511811023723 ) ) ;
#3103 = AXIS2_PLACEMENT_3D ( 'NONE', #25732, #1857, #21496 ) ;
#3104 = CARTESIAN_POINT ( 'NONE',  ( -0.06880207798751750148, 0.1968503937007873850, -3.587883383884437727 ) ) ;
#3105 = APPLICATION_CONTEXT ( 'automotive_design' ) ;
#3106 = ADVANCED_FACE ( 'NONE', ( #26499 ), #24657, .T. ) ;
#3107 = DIRECTION ( 'NONE',  ( 0.000000000000000000, -1.000000000000000000, 0.000000000000000000 ) ) ;
#3108 = ORIENTED_EDGE ( 'NONE', *, *, #14866, .F. ) ;
#3109 = EDGE_CURVE ( 'NONE', #9597, #14042, #11187, .T. ) ;
#3110 = MECHANICAL_DESIGN_GEOMETRIC_PRESENTATION_REPRESENTATION (  '', ( #18434 ), #11231 ) ;
#3111 = CARTESIAN_POINT ( 'NONE',  ( 0.003937007874015826907, 8.142711329854796413E-18, 0.1023622047244094474 ) ) ;
#3112 = CARTESIAN_POINT ( 'NONE',  ( 0.7430739993161732393, 0.4424178910903722728, -0.3641321082570454504 ) ) ;
#3113 = DIRECTION ( 'NONE',  ( -1.000000000000000000, 0.000000000000000000, 0.000000000000000000 ) ) ;
#3114 = ORIENTED_EDGE ( 'NONE', *, *, #27574, .T. ) ;
#3115 = EDGE_CURVE ( 'NONE', #27881, #10521, #9696, .T. ) ;
#3116 = B_SPLINE_CURVE_WITH_KNOTS ( 'NONE', 3,
 ( #10774, #17276, #11053, #10625, #19392, #13308 ),
 .UNSPECIFIED., .F., .F.,
 ( 4, 2, 4 ),
 ( 0.000000000000000000, 0.2500000000000000000, 0.5000000000000000000 ),
 .UNSPECIFIED. ) ;
#3117 = VERTEX_POINT ( 'NONE', #26939 ) ;
#3118 = CARTESIAN_POINT ( 'NONE',  ( -0.1078280746904014958, -0.3175540113612295157, 1.973425196850393970 ) ) ;
#3119 = CARTESIAN_POINT ( 'NONE',  ( 0.4889536969034951053, 0.06441834428467130280, -1.550196850393700920 ) ) ;
#3120 = EDGE_CURVE ( 'NONE', #7099, #13627, #22918, .T. ) ;
#3121 = CARTESIAN_POINT ( 'NONE',  ( -0.4681308612729627172, -0.1074986424507606841, 0.2362204724409447676 ) ) ;
#3122 = AXIS2_PLACEMENT_3D ( 'NONE', #20332, #24693, #13985 ) ;
#3123 = CARTESIAN_POINT ( 'NONE',  ( 0.07214854559197284023, -0.5476281405333195407, 0.9202755905511811330 ) ) ;
#3124 = CARTESIAN_POINT ( 'NONE',  ( -0.4783464566929133688, -0.4724409448818898127, -0.8182917201112815953 ) ) ;
#3125 = CONICAL_SURFACE ( 'NONE', #24330, 0.2938622683360631593, 0.2617993874999998138 ) ;
#3126 = CARTESIAN_POINT ( 'NONE',  ( -4.821283464566928349E-18, 0.000000000000000000, -0.2834645669291338543 ) ) ;
#3127 = CARTESIAN_POINT ( 'NONE',  ( 0.09855118063547671503, -0.3667122560601320247, -3.100567304031763172 ) ) ;
#3128 = DIRECTION ( 'NONE',  ( 0.4999999999999993894, 6.123233995736758640E-17, -0.8660254037844389297 ) ) ;
#3129 = CARTESIAN_POINT ( 'NONE',  ( 0.1709077104829875848, -0.4707213777573787672, 0.2574819596263889787 ) ) ;
#3130 = FACE_OUTER_BOUND ( 'NONE', #2150, .T. ) ;
#3131 = CARTESIAN_POINT ( 'NONE',  ( 0.3222028160008074682, 0.3833711078595924970, 0.2574819596263889787 ) ) ;
#3132 = VERTEX_POINT ( 'NONE', #22237 ) ;
#3133 = EDGE_CURVE ( 'NONE', #12001, #8922, #22523, .T. ) ;
#3134 = LENGTH_MEASURE_WITH_UNIT ( LENGTH_MEASURE( 0.02539999999999999897 ), #2220 ) ;
#3135 = DIRECTION ( 'NONE',  ( 0.000000000000000000, 0.000000000000000000, 1.000000000000000000 ) ) ;
#3136 = CARTESIAN_POINT ( 'NONE',  ( 0.000000000000000000, 0.000000000000000000, 0.1377952755905511584 ) ) ;
#3137 = EDGE_CURVE ( 'NONE', #21046, #13737, #4429, .T. ) ;
#3138 = ORIENTED_EDGE ( 'NONE', *, *, #23236, .F. ) ;
#3139 = AXIS2_PLACEMENT_3D ( 'NONE', #11704, #2936, #20846 ) ;
#3140 = CARTESIAN_POINT ( 'NONE',  ( -0.0001724821237274320063, 0.3771653543307086909, 0.07637549214372835182 ) ) ;
#3141 = ORIENTED_EDGE ( 'NONE', *, *, #21514, .F. ) ;
#3142 = CARTESIAN_POINT ( 'NONE',  ( 0.0006443779181925812262, 0.4960456921221567672, 0.2989974301410669444 ) ) ;
#3143 = AXIS2_PLACEMENT_3D ( 'NONE', #25557, #10283, #3501 ) ;
#3144 = CARTESIAN_POINT ( 'NONE',  ( -0.1608692170994283632, -0.4408576787418519993, 0.1992142434433716580 ) ) ;
#3145 = LINE ( 'NONE', #27043, #2416 ) ;
#3146 = LINE ( 'NONE', #11777, #7662 ) ;
#3147 = FACE_OUTER_BOUND ( 'NONE', #4581, .T. ) ;
#3148 = EDGE_LOOP ( 'NONE', ( #27180, #1682, #9509, #8478, #4115, #23919 ) ) ;
#3149 = CARTESIAN_POINT ( 'NONE',  ( -0.6711032387266614441, -0.1523958994813200962, 0.1322834645669291320 ) ) ;
#3150 = AXIS2_PLACEMENT_3D ( 'NONE', #6820, #24869, #11879 ) ;
#3151 = DIRECTION ( 'NONE',  ( 0.000000000000000000, 0.000000000000000000, 1.000000000000000000 ) ) ;
#3152 = EDGE_CURVE ( 'NONE', #6711, #11971, #24912, .T. ) ;
#3153 = VERTEX_POINT ( 'NONE', #3149 ) ;
#3154 = CARTESIAN_POINT ( 'NONE',  ( 0.04928467685643810742, 0.3740848232703744003, -3.100567304031763172 ) ) ;
#3155 = DIRECTION ( 'NONE',  ( -1.000000000000000000, 0.000000000000000000, 0.000000000000000000 ) ) ;
#3156 = CARTESIAN_POINT ( 'NONE',  ( 0.3722026523000413478, 4.558167867734008572E-17, -0.1756889763779527769 ) ) ;
#3157 = PRODUCT_DEFINITION_CONTEXT ( 'detailed design', #6031, 'design' ) ;
#3158 = ORIENTED_EDGE ( 'NONE', *, *, #8802, .T. ) ;
#3159 = CARTESIAN_POINT ( 'NONE',  ( 0.3858397471888842523, 0.2228126397719887297, -1.934055118110236338 ) ) ;
#3160 = VERTEX_POINT ( 'NONE', #11502 ) ;
#3161 = CARTESIAN_POINT ( 'NONE',  ( -0.3338887748335567229, -1.257773430019720307, -0.7637447580504644895 ) ) ;
#3162 = DIRECTION ( 'NONE',  ( 0.7071067818211385081, 0.7071067805519564153, -8.659560554583433905E-17 ) ) ;
#3163 = CARTESIAN_POINT ( 'NONE',  ( 0.3382184156732089830, -0.3855916753051465973, 1.766732283464566899 ) ) ;
#3164 = CARTESIAN_POINT ( 'NONE',  ( 0.6055690743987126590, 0.2581485381169802973, 0.4471263839182408883 ) ) ;
#3165 = AXIS2_PLACEMENT_3D ( 'NONE', #26491, #11954, #22410 ) ;
#3166 = CARTESIAN_POINT ( 'NONE',  ( 0.2488091035917030791, 0.2836590635674509642, -3.100567304031764948 ) ) ;
#3167 = B_SPLINE_CURVE_WITH_KNOTS ( 'NONE', 3,
 ( #10551, #16646, #19174, #17064, #23013, #27385 ),
 .UNSPECIFIED., .F., .F.,
 ( 4, 2, 4 ),
 ( 0.000000000000000000, 0.2500000000000000000, 0.5000000000000000000 ),
 .UNSPECIFIED. ) ;
#3168 = DIRECTION ( 'NONE',  ( 0.000000000000000000, -1.000000000000000000, 0.000000000000000000 ) ) ;
#3169 = DIRECTION ( 'NONE',  ( 0.000000000000000000, 0.000000000000000000, 1.000000000000000000 ) ) ;
#3170 = EDGE_CURVE ( 'NONE', #22329, #8047, #3984, .T. ) ;
#3171 = ORIENTED_EDGE ( 'NONE', *, *, #3875, .F. ) ;
#3172 = VERTEX_POINT ( 'NONE', #20257 ) ;
#3173 = ADVANCED_FACE ( 'NONE', ( #17968 ), #22023, .T. ) ;
#3174 = CARTESIAN_POINT ( 'NONE',  ( -0.3558329076891611487, -0.7201416780480096591, -0.6679878162024859289 ) ) ;
#3175 = CARTESIAN_POINT ( 'NONE',  ( -6.092417322834646079E-17, 0.1968503937007874127, -3.272637795275590733 ) ) ;
#3176 = ORIENTED_EDGE ( 'NONE', *, *, #19126, .T. ) ;
#3177 = CARTESIAN_POINT ( 'NONE',  ( -0.1152775731717027019, -0.4303822302053992854, -1.934055118110236338 ) ) ;
#3178 = ORIENTED_EDGE ( 'NONE', *, *, #23388, .T. ) ;
#3179 = EDGE_LOOP ( 'NONE', ( #24269, #12231, #18979, #26878, #16717, #1284, #25406, #4482, #12261, #20323, #15391, #27067, #5957 ) ) ;
#3180 = CARTESIAN_POINT ( 'NONE',  ( 0.5118110236220472231, 6.267877318470705905E-17, 1.953740157480315043 ) ) ;
#3181 = FACE_BOUND ( 'NONE', #12605, .T. ) ;
#3182 = CIRCLE ( 'NONE', #20802, 0.1003956692913386267 ) ;
#3183 = CARTESIAN_POINT ( 'NONE',  ( -0.3213305936751693626, 0.1584254766472210918, -3.115157480314960647 ) ) ;
#3184 = CARTESIAN_POINT ( 'NONE',  ( -0.07874015748031502893, 0.1968503937007873850, -3.262343610818749795 ) ) ;
#3185 = CARTESIAN_POINT ( 'NONE',  ( -1.012503259137575512E-16, -0.8267716535433071723, 0.02362204724409448786 ) ) ;
#3186 = CYLINDRICAL_SURFACE ( 'NONE', #8980, 0.5570866141732283561 ) ;
#3187 = CIRCLE ( 'NONE', #25763, 0.09143349766193348271 ) ;
#3188 = CARTESIAN_POINT ( 'NONE',  ( 0.000000000000000000, 0.000000000000000000, 0.2362204724409449064 ) ) ;
#3189 = CARTESIAN_POINT ( 'NONE',  ( 0.6241612306998541859, 0.1093779649449431318, 0.1061598535669114746 ) ) ;
#3190 = CARTESIAN_POINT ( 'NONE',  ( 0.09187177619658809524, -0.3429980251342298336, 1.953740157480315043 ) ) ;
#3191 = CARTESIAN_POINT ( 'NONE',  ( -0.6993003464547263848, -0.1604063846365767210, 0.3122824329331324034 ) ) ;
#3192 = CARTESIAN_POINT ( 'NONE',  ( -0.5379168165870276130, -0.3108204284649299098, 0.09684793308443542803 ) ) ;
#3193 = CARTESIAN_POINT ( 'NONE',  ( 0.000000000000000000, 0.000000000000000000, 0.5905511811023621549 ) ) ;
#3194 = DIRECTION ( 'NONE',  ( 0.000000000000000000, 1.000000000000000000, 0.000000000000000000 ) ) ;
#3195 = DIRECTION ( 'NONE',  ( 0.000000000000000000, 1.000000000000000000, 0.000000000000000000 ) ) ;
#3196 = CARTESIAN_POINT ( 'NONE',  ( 0.2663596103035608120, 0.4612490782035171266, 1.747047244094488194 ) ) ;
#3197 = CARTESIAN_POINT ( 'NONE',  ( 0.1506723201675407575, 0.000000000000000000, 0.000000000000000000 ) ) ;
#3198 = CARTESIAN_POINT ( 'NONE',  ( 0.3382184156732163660, 0.3855916753051394363, 1.747047244094488194 ) ) ;
#3199 = EDGE_LOOP ( 'NONE', ( #18507, #7887, #23739, #14230, #25167, #506, #9319, #4343, #12090, #12890, #24965, #10457 ) ) ;
#3200 = FACE_BOUND ( 'NONE', #16559, .T. ) ;
#3201 = VERTEX_POINT ( 'NONE', #18103 ) ;
#3202 = EDGE_CURVE ( 'NONE', #24677, #19192, #17913, .T. ) ;
#3203 = CARTESIAN_POINT ( 'NONE',  ( 0.3149606299212598381, 0.3346456692913385988, 0.000000000000000000 ) ) ;
#3204 = DIRECTION ( 'NONE',  ( 0.000000000000000000, 0.000000000000000000, -1.000000000000000000 ) ) ;
#3205 = ADVANCED_FACE ( 'NONE', ( #15750 ), #24270, .T. ) ;
#3206 = DIRECTION ( 'NONE',  ( 0.000000000000000000, 1.000000000000000000, 0.000000000000000000 ) ) ;
#3207 = EDGE_LOOP ( 'NONE', ( #5503, #12814, #14113, #25331 ) ) ;
#3208 = ORIENTED_EDGE ( 'NONE', *, *, #21724, .F. ) ;
#3209 = AXIS2_PLACEMENT_3D ( 'NONE', #3734, #14648, #3882 ) ;
#3210 = CARTESIAN_POINT ( 'NONE',  ( -0.1585706980422252055, -0.4669911931914896841, -1.569881889763779625 ) ) ;
#3211 = CARTESIAN_POINT ( 'NONE',  ( -0.09842519685039370636, -0.07874015748031495954, -0.04546065111729338803 ) ) ;
#3212 = EDGE_LOOP ( 'NONE', ( #10838, #26594, #26632, #8189 ) ) ;
#3213 = VERTEX_POINT ( 'NONE', #26893 ) ;
#3214 = ORIENTED_EDGE ( 'NONE', *, *, #15264, .T. ) ;
#3215 = CARTESIAN_POINT ( 'NONE',  ( 0.000000000000000000, 0.000000000000000000, -4.330708661396418080 ) ) ;
#3216 = CARTESIAN_POINT ( 'NONE',  ( 0.000000000000000000, 0.5905511811023621549, 0.000000000000000000 ) ) ;
#3217 = CARTESIAN_POINT ( 'NONE',  ( 4.701028524955307180E-18, 0.4232283464566928832, 0.06102165354330708891 ) ) ;
#3218 = DIRECTION ( 'NONE',  ( -0.9790454724845842893, -0.1018208755700880375, 0.1763589297585410332 ) ) ;
#3219 = VECTOR ( 'NONE', #21211, 39.37007874015748143 ) ;
#3220 = DIRECTION ( 'NONE',  ( 0.000000000000000000, 0.000000000000000000, 1.000000000000000000 ) ) ;
#3221 = ADVANCED_FACE ( 'NONE', ( #13904 ), #18385, .F. ) ;
#3222 = ORIENTED_EDGE ( 'NONE', *, *, #18065, .T. ) ;
#3223 = CARTESIAN_POINT ( 'NONE',  ( -1.197070535079588716, 0.4724409448818898127, -1.078960298859116707 ) ) ;
#3224 = FACE_OUTER_BOUND ( 'NONE', #18819, .T. ) ;
#3225 = DIRECTION ( 'NONE',  ( 1.000000000000000000, 0.000000000000000000, 0.000000000000000000 ) ) ;
#3226 = CARTESIAN_POINT ( 'NONE',  ( -0.3916295560419718602, 0.3131429078191630411, 0.1643955689142584109 ) ) ;
#3227 = CARTESIAN_POINT ( 'NONE',  ( -0.3263749705684267921, -0.1890319631540330891, 0.07637795275590551769 ) ) ;
#3228 = ADVANCED_FACE ( 'NONE', ( #5573 ), #19299, .T. ) ;
#3229 = ORIENTED_EDGE ( 'NONE', *, *, #19328, .T. ) ;
#3230 = DIRECTION ( 'NONE',  ( 0.000000000000000000, -0.8660254037844388186, 0.4999999999999998890 ) ) ;
#3231 = AXIS2_PLACEMENT_3D ( 'NONE', #10033, #1845, #10310 ) ;
#3232 = VERTEX_POINT ( 'NONE', #22378 ) ;
#3233 = AXIS2_PLACEMENT_3D ( 'NONE', #5793, #12422, #5933 ) ;
#3234 = CARTESIAN_POINT ( 'NONE',  ( -0.08530183727034115759, -0.03937007874015747977, 0.06819097667594049839 ) ) ;
#3235 = CARTESIAN_POINT ( 'NONE',  ( -0.8725268807032540153, 0.000000000000000000, -1.052618110236220428 ) ) ;
#3236 = CARTESIAN_POINT ( 'NONE',  ( -0.06296589279854382382, 0.1968503937007873850, -3.596617852270226567 ) ) ;
#3237 = CONICAL_SURFACE ( 'NONE', #23126, 0.2012500529900838608, 1.047197550000000144 ) ;
#3238 = DIRECTION ( 'NONE',  ( -0.000000000000000000, -0.000000000000000000, -1.000000000000000000 ) ) ;
#3239 = VERTEX_POINT ( 'NONE', #12065 ) ;
#3240 = CIRCLE ( 'NONE', #8236, 0.06200787401574805319 ) ;
#3241 = FILL_AREA_STYLE_COLOUR ( '', #9417 ) ;
#3242 = CARTESIAN_POINT ( 'NONE',  ( -0.2395669291338582696, 0.000000000000000000, -0.4724409448818898127 ) ) ;
#3243 = CARTESIAN_POINT ( 'NONE',  ( 0.4895462770358314786, 1.042587244177472394, -0.2949132003433866389 ) ) ;
#3244 = ADVANCED_FACE ( 'NONE', ( #18257 ), #7258, .F. ) ;
#3245 = DIRECTION ( 'NONE',  ( 0.000000000000000000, 0.000000000000000000, -1.000000000000000000 ) ) ;
#3246 = LINE ( 'NONE', #11888, #10154 ) ;
#3247 = VERTEX_POINT ( 'NONE', #22802 ) ;
#3248 = ORIENTED_EDGE ( 'NONE', *, *, #16548, .T. ) ;
#3249 = CARTESIAN_POINT ( 'NONE',  ( 0.000000000000000000, 0.3771653543307086909, 0.2374015748031496065 ) ) ;
#3250 = CARTESIAN_POINT ( 'NONE',  ( 0.3905379133858267737, -0.2805118110236220486, 0.4858607088160724063 ) ) ;
#3251 = CARTESIAN_POINT ( 'NONE',  ( 0.1585706980422384171, -0.4669911931914537129, -1.550196850393700920 ) ) ;
#3252 = AXIS2_PLACEMENT_3D ( 'NONE', #5989, #19250, #27453 ) ;
#3253 = DIRECTION ( 'NONE',  ( 0.000000000000000000, 0.000000000000000000, 1.000000000000000000 ) ) ;
#3254 = AXIS2_PLACEMENT_3D ( 'NONE', #4997, #919, #13619 ) ;
#3255 = CARTESIAN_POINT ( 'NONE',  ( 0.1429116519061227053, -0.5335524835332334792, 0.9202755905511811330 ) ) ;
#3256 = CARTESIAN_POINT ( 'NONE',  ( 0.000000000000000000, 0.000000000000000000, 0.1771653543307086520 ) ) ;
#3257 = EDGE_CURVE ( 'NONE', #372, #13858, #19762, .T. ) ;
#3258 = FACE_OUTER_BOUND ( 'NONE', #14398, .T. ) ;
#3259 = CARTESIAN_POINT ( 'NONE',  ( -0.06894484415077309358, 0.05111597790490104293, -0.4724409448818898127 ) ) ;
#3260 = EDGE_CURVE ( 'NONE', #24896, #24517, #12074, .T. ) ;
#3261 = DIRECTION ( 'NONE',  ( -1.000000000000000000, 0.000000000000000000, 0.000000000000000000 ) ) ;
#3262 = AXIS2_PLACEMENT_3D ( 'NONE', #6731, #2738, #388 ) ;
#3263 = CARTESIAN_POINT ( 'NONE',  ( 0.1522836969735571200, -0.4941010236220468865, 0.01864847287710767396 ) ) ;
#3264 = ORIENTED_EDGE ( 'NONE', *, *, #19902, .T. ) ;
#3265 = EDGE_CURVE ( 'NONE', #5138, #26931, #25605, .T. ) ;
#3266 = DIRECTION ( 'NONE',  ( -0.2036417511401763802, 0.4895227362422922557, 0.8478782506317883438 ) ) ;
#3267 = CARTESIAN_POINT ( 'NONE',  ( -0.1379032889621888969, 0.5144765700550301135, 1.747047244094488194 ) ) ;
#3268 = FILL_AREA_STYLE ('',( #26447 ) ) ;
#3269 = DIRECTION ( 'NONE',  ( 0.000000000000000000, 1.000000000000000000, 0.000000000000000000 ) ) ;
#3270 = ORIENTED_EDGE ( 'NONE', *, *, #16719, .F. ) ;
#3271 = EDGE_LOOP ( 'NONE', ( #24542, #16400, #27074, #1358 ) ) ;
#3272 = DIRECTION ( 'NONE',  ( 0.7071067811865475727, -0.7071067811865475727, 0.000000000000000000 ) ) ;
#3273 = FACE_BOUND ( 'NONE', #23803, .T. ) ;
#3275 = CARTESIAN_POINT ( 'NONE',  ( 0.3937007874015748254, -5.011764252456519698E-17, -0.07578740157480315376 ) ) ;
#3276 = ORIENTED_EDGE ( 'NONE', *, *, #6822, .F. ) ;
#3277 = CIRCLE ( 'NONE', #19540, 0.7283464566929134243 ) ;
#3278 = CARTESIAN_POINT ( 'NONE',  ( -0.3149606299212598381, 0.000000000000000000, 0.000000000000000000 ) ) ;
#3279 = ORIENTED_EDGE ( 'NONE', *, *, #10114, .F. ) ;
#3280 = CIRCLE ( 'NONE', #22700, 0.1771653543307086798 ) ;
#3281 = DIRECTION ( 'NONE',  ( -0.5000000010362850578, -0.8660254031861391866, -1.060575237992201443E-16 ) ) ;
#3282 = CARTESIAN_POINT ( 'NONE',  ( 0.5383572925355968319, -0.3100567972183901899, 0.09685039370078740717 ) ) ;
#3283 = CARTESIAN_POINT ( 'NONE',  ( 0.1504366439317612048, -0.2089021884548363517, 0.4380456861425212622 ) ) ;
#3284 = DIRECTION ( 'NONE',  ( 0.000000000000000000, 0.000000000000000000, 1.000000000000000000 ) ) ;
#3285 = DIRECTION ( 'NONE',  ( -1.000000000000000000, 0.000000000000000000, 0.000000000000000000 ) ) ;
#3286 = DIRECTION ( 'NONE',  ( 1.000000000000000000, 0.000000000000000000, 0.000000000000000000 ) ) ;
#3287 = DIRECTION ( 'NONE',  ( 1.000000000000000000, 0.000000000000000000, 0.000000000000000000 ) ) ;
#3288 = CARTESIAN_POINT ( 'NONE',  ( 0.6299212598425196763, 0.4076750295275590741, 0.000000000000000000 ) ) ;
#3289 = ORIENTED_EDGE ( 'NONE', *, *, #7803, .T. ) ;
#3290 = CARTESIAN_POINT ( 'NONE',  ( -0.3644697409450258219, -0.09762295995070061072, -3.100567304031765836 ) ) ;
#3291 = AXIS2_PLACEMENT_3D ( 'NONE', #15788, #13949, #815 ) ;
#3292 = ( NAMED_UNIT ( * ) PLANE_ANGLE_UNIT ( ) SI_UNIT ( $, .RADIAN. ) ) ;
#3293 = VERTEX_POINT ( 'NONE', #9801 ) ;
#3294 = CARTESIAN_POINT ( 'NONE',  ( -0.3996230174612653285, -0.1970259548082108347, -1.934055118110236338 ) ) ;
#3295 = EDGE_CURVE ( 'NONE', #12667, #24639, #7116, .T. ) ;
#3296 = ADVANCED_FACE ( 'NONE', ( #22949, #10636 ), #4016, .T. ) ;
#3297 = AXIS2_PLACEMENT_3D ( 'NONE', #2589, #11212, #19836 ) ;
#3298 = ORIENTED_EDGE ( 'NONE', *, *, #16372, .F. ) ;
#3299 = ORIENTED_EDGE ( 'NONE', *, *, #24840, .T. ) ;
#3300 = CARTESIAN_POINT ( 'NONE',  ( -0.4280150452258433269, -0.8372280483532893447, -0.07105027534967854608 ) ) ;
#3301 = FACE_OUTER_BOUND ( 'NONE', #4635, .T. ) ;
#3302 = CARTESIAN_POINT ( 'NONE',  ( 0.3512268162760394108, 0.4004221243553300891, 1.747047244094488194 ) ) ;
#3303 = ( NAMED_UNIT ( * ) SI_UNIT ( $, .STERADIAN. ) SOLID_ANGLE_UNIT ( ) ) ;
#3304 = CARTESIAN_POINT ( 'NONE',  ( 0.2488091035916884242, -0.2836590635674675620, -3.100567304031759175 ) ) ;
#3305 = CIRCLE ( 'NONE', #7399, 0.3070866141732283561 ) ;
#3306 = ORIENTED_EDGE ( 'NONE', *, *, #13358, .T. ) ;
#3307 = DIRECTION ( 'NONE',  ( 0.000000000000000000, 0.000000000000000000, -1.000000000000000000 ) ) ;
#3308 = CARTESIAN_POINT ( 'NONE',  ( -0.2602238532265429005, 0.000000000000000000, -0.07874015748031495954 ) ) ;
#3309 = EDGE_CURVE ( 'NONE', #11845, #25113, #17201, .T. ) ;
#3310 = ORIENTED_EDGE ( 'NONE', *, *, #2485, .T. ) ;
#3311 = CARTESIAN_POINT ( 'NONE',  ( -0.4300685960020619314, -0.5253395418799321481, -0.4276959590273259337 ) ) ;
#3312 = CARTESIAN_POINT ( 'NONE',  ( -0.03937007874015747977, 0.000000000000000000, 0.000000000000000000 ) ) ;
#3313 = ORIENTED_EDGE ( 'NONE', *, *, #20255, .F. ) ;
#3314 = CARTESIAN_POINT ( 'NONE',  ( 0.4446020952038907681, 0.02909913904662021419, -1.934055118110236338 ) ) ;
#3315 = ORIENTED_EDGE ( 'NONE', *, *, #27216, .T. ) ;
#3316 = ORIENTED_EDGE ( 'NONE', *, *, #25771, .F. ) ;
#3317 = DIRECTION ( 'NONE',  ( -1.000000000000000000, 0.000000000000000000, 0.000000000000000000 ) ) ;
#3318 = CARTESIAN_POINT ( 'NONE',  ( 0.2395669291338582696, 2.933848729453403498E-17, 0.000000000000000000 ) ) ;
#3319 = TOROIDAL_SURFACE ( 'NONE', #4680, 0.6102362204724409711, 0.1299212598425196763 ) ;
#3320 = CARTESIAN_POINT ( 'NONE',  ( 0.1584254766472226184, 0.3213305936751399972, -3.115157480314960647 ) ) ;
#3321 = CARTESIAN_POINT ( 'NONE',  ( 0.2775852647713620280, -0.4816145447621893450, 0.9202755905511812440 ) ) ;
#3322 = CARTESIAN_POINT ( 'NONE',  ( 0.5885985490145342336, 0.9326256249715371149, -0.1629194618731351907 ) ) ;
#3323 = CARTESIAN_POINT ( 'NONE',  ( -2.685748425196850164E-17, 0.000000000000000000, -3.745078740157480546 ) ) ;
#3325 = EDGE_CURVE ( 'NONE', #25692, #23663, #26075, .T. ) ;
#3324 = AXIS2_PLACEMENT_3D ( 'NONE', #16852, #21074, #18807 ) ;
#3326 = CARTESIAN_POINT ( 'NONE',  ( 0.2924088307484721261, -0.1685339107540413384, 1.973425196850394192 ) ) ;
#3327 = AXIS2_PLACEMENT_3D ( 'NONE', #25026, #20652, #14305 ) ;
#3328 = CARTESIAN_POINT ( 'NONE',  ( 0.03008364706454716778, 0.1136516277932340530, -0.1968503937007874127 ) ) ;
#3329 = EDGE_CURVE ( 'NONE', #8587, #13219, #1714, .T. ) ;
#3330 = VERTEX_POINT ( 'NONE', #27325 ) ;
#3331 = DIRECTION ( 'NONE',  ( 1.000000000000000000, 0.000000000000000000, 0.000000000000000000 ) ) ;
#3332 = CARTESIAN_POINT ( 'NONE',  ( 0.000000000000000000, 0.000000000000000000, -1.092739370078740131E-17 ) ) ;
#3333 = CARTESIAN_POINT ( 'NONE',  ( 0.3217486617182078734, 0.3837523410419874659, 0.09684793308443542803 ) ) ;
#3334 = CARTESIAN_POINT ( 'NONE',  ( 1.857656692913385893E-16, 0.6193720790381457286, 7.649715443242610847E-17 ) ) ;
#3335 = ORIENTED_EDGE ( 'NONE', *, *, #7386, .T. ) ;
#3336 = DIRECTION ( 'NONE',  ( 0.000000000000000000, 0.000000000000000000, -1.000000000000000000 ) ) ;
#3337 = CARTESIAN_POINT ( 'NONE',  ( 0.06957181182498554939, 0.5280699926562867352, 1.747047244094488194 ) ) ;
#3338 = CARTESIAN_POINT ( 'NONE',  ( -0.5085118447801436625, -0.06699507805368999647, 1.766732283464566899 ) ) ;
#3339 = AXIS2_PLACEMENT_3D ( 'NONE', #27556, #6091, #1969 ) ;
#3340 = ORIENTED_EDGE ( 'NONE', *, *, #4961, .F. ) ;
#3341 = DIRECTION ( 'NONE',  ( 1.000000000000000000, 0.000000000000000000, 0.000000000000000000 ) ) ;
#3342 = ORIENTED_EDGE ( 'NONE', *, *, #949, .T. ) ;
#3343 = EDGE_CURVE ( 'NONE', #8702, #26390, #17501, .T. ) ;
#3344 = CARTESIAN_POINT ( 'NONE',  ( 0.3334645669291338987, -1.269546425348450747, -0.8304542831125020230 ) ) ;
#3345 = CARTESIAN_POINT ( 'NONE',  ( -0.0005789221761808661720, 0.4692909815006409691, 0.1992125984251968684 ) ) ;
#3346 = ADVANCED_FACE ( 'NONE', ( #23521 ), #7581, .T. ) ;
#3347 = ORIENTED_EDGE ( 'NONE', *, *, #8429, .F. ) ;
#3348 = EDGE_LOOP ( 'NONE', ( #21676, #27774, #19131, #2459, #17124, #23248 ) ) ;
#3349 = CIRCLE ( 'NONE', #14675, 0.1003956692913385990 ) ;
#3350 = CARTESIAN_POINT ( 'NONE',  ( 0.1585706980422248169, 0.4669911931914899617, -1.569881889763779625 ) ) ;
#3351 = EDGE_LOOP ( 'NONE', ( #1612, #533, #23574, #1035 ) ) ;
#3352 = ORIENTED_EDGE ( 'NONE', *, *, #1409, .F. ) ;
#3353 = CARTESIAN_POINT ( 'NONE',  ( 0.4931105264837953306, 0.08735026989778603423, 0.2574819596263889787 ) ) ;
#3354 = CARTESIAN_POINT ( 'NONE',  ( -0.2423050875943940918, 0.2890362931940642088, 0.1992150590373740204 ) ) ;
#3355 = DIRECTION ( 'NONE',  ( 1.000000000000000000, 0.000000000000000000, 0.000000000000000000 ) ) ;
#3356 = CIRCLE ( 'NONE', #21900, 0.07874015748031489015 ) ;
#3357 = EDGE_LOOP ( 'NONE', ( #19208, #4870, #20216, #2165 ) ) ;
#3358 = DIRECTION ( 'NONE',  ( 0.000000000000000000, 1.000000000000000000, 0.000000000000000000 ) ) ;
#3359 = EDGE_CURVE ( 'NONE', #24341, #18758, #1276, .T. ) ;
#3360 = UNCERTAINTY_MEASURE_WITH_UNIT (LENGTH_MEASURE( 1.000000000000000082E-05 ), #12173, 'distance_accuracy_value', 'NONE') ;
#3361 = ORIENTED_EDGE ( 'NONE', *, *, #23536, .T. ) ;
#3362 = DIRECTION ( 'NONE',  ( 0.000000000000000000, 0.000000000000000000, 1.000000000000000000 ) ) ;
#3363 = CIRCLE ( 'NONE', #15129, 0.2938622683360631593 ) ;
#3364 = CIRCLE ( 'NONE', #24588, 0.4685039370078740717 ) ;
#3365 = CARTESIAN_POINT ( 'NONE',  ( -0.3935368318888682326, 0.3024344094364739277, -1.569881889763779625 ) ) ;
#3366 = DIRECTION ( 'NONE',  ( -1.000000000000000000, 0.000000000000000000, 0.000000000000000000 ) ) ;
#3367 = ORIENTED_EDGE ( 'NONE', *, *, #11351, .F. ) ;
#3368 = VERTEX_POINT ( 'NONE', #14337 ) ;
#3369 = ( CONVERSION_BASED_UNIT ( 'INCH', #1148 ) LENGTH_UNIT ( ) NAMED_UNIT ( #6369 ) ) ;
#3370 = CONICAL_SURFACE ( 'NONE', #2510, 0.4537419570391968415, 1.365720138124999927 ) ;
#3371 = VERTEX_POINT ( 'NONE', #7973 ) ;
#3372 = DIRECTION ( 'NONE',  ( 1.000000000000000000, 0.000000000000000000, 0.000000000000000000 ) ) ;
#3373 = CARTESIAN_POINT ( 'NONE',  ( 8.741913385826771462E-17, 0.1673228346456692994, 0.000000000000000000 ) ) ;
#3374 = VERTEX_POINT ( 'NONE', #10356 ) ;
#3375 = DIRECTION ( 'NONE',  ( -1.224646799147353207E-16, 1.000000000000000000, 0.000000000000000000 ) ) ;
#3376 = DIRECTION ( 'NONE',  ( 1.000000000000000000, 0.000000000000000000, 0.000000000000000000 ) ) ;
#3377 = ORIENTED_EDGE ( 'NONE', *, *, #26972, .F. ) ;
#3378 = EDGE_CURVE ( 'NONE', #23608, #401, #8941, .T. ) ;
#3379 = VECTOR ( 'NONE', #4006, 39.37007874015748854 ) ;
#3380 = ( NAMED_UNIT ( * ) PLANE_ANGLE_UNIT ( ) SI_UNIT ( $, .RADIAN. ) ) ;
#3381 = CIRCLE ( 'NONE', #6159, 0.06200787401574805319 ) ;
#3382 = CARTESIAN_POINT ( 'NONE',  ( 0.000000000000000000, 0.000000000000000000, -0.2204724409448818867 ) ) ;
#3383 = CARTESIAN_POINT ( 'NONE',  ( -0.4954247181591361904, -0.1327957795771543825, -1.550196850393700254 ) ) ;
#3384 = CIRCLE ( 'NONE', #22817, 0.4173228346456693272 ) ;
#3385 = FACE_BOUND ( 'NONE', #2357, .T. ) ;
#3386 = CARTESIAN_POINT ( 'NONE',  ( -0.1579154690106709391, -0.4355388305871915056, 0.1494804571213769195 ) ) ;
#3387 = EDGE_CURVE ( 'NONE', #20876, #16172, #1888, .T. ) ;
#3388 = CARTESIAN_POINT ( 'NONE',  ( 0.4954219348937308198, -0.1327952259508279609, -1.550196850393700476 ) ) ;
#3389 = ORIENTED_EDGE ( 'NONE', *, *, #2969, .F. ) ;
#3390 = VERTEX_POINT ( 'NONE', #10494 ) ;
#3391 = CARTESIAN_POINT ( 'NONE',  ( -0.2904160862623646477, -0.1677079028045411757, 1.973425196850393970 ) ) ;
#3392 = CARTESIAN_POINT ( 'NONE',  ( 0.3855916753034099864, -0.3382184156749167836, -1.550196850393700920 ) ) ;
#3393 = CARTESIAN_POINT ( 'NONE',  ( -0.4681308612729632168, -0.1074986424507606286, 0.2529987172304648535 ) ) ;
#3394 = CARTESIAN_POINT ( 'NONE',  ( 0.4783323773986672967, -0.2762247810518773106, 0.9202755905511811330 ) ) ;
#3395 = DIRECTION ( 'NONE',  ( 1.000000000000000000, 0.000000000000000000, 0.000000000000000000 ) ) ;
#3396 = MANIFOLD_SOLID_BREP ( 'Barrel Cam', #16864 ) ;
#3397 = DIRECTION ( 'NONE',  ( 0.000000000000000000, 0.000000000000000000, 1.000000000000000000 ) ) ;
#3398 = ORIENTED_EDGE ( 'NONE', *, *, #9003, .T. ) ;
#3399 = DIRECTION ( 'NONE',  ( 0.000000000000000000, 0.000000000000000000, 1.000000000000000000 ) ) ;
#3400 = CARTESIAN_POINT ( 'NONE',  ( -0.3252100150720461658, 0.3707612262532960501, -1.569881889763779625 ) ) ;
#3401 = CARTESIAN_POINT ( 'NONE',  ( 0.000000000000000000, 0.5610236220472440971, 0.3543307086614173040 ) ) ;
#3402 = CIRCLE ( 'NONE', #20119, 0.4807043897637795493 ) ;
#3403 = DIRECTION ( 'NONE',  ( -0.000000000000000000, -1.000000000000000000, -0.000000000000000000 ) ) ;
#3404 = CARTESIAN_POINT ( 'NONE',  ( 0.5314960629921260393, 0.000000000000000000, 1.747047244094488194 ) ) ;
#3405 = CARTESIAN_POINT ( 'NONE',  ( 0.3268939675028499914, -0.1881330340946397728, 0.07637795275590551769 ) ) ;
#3406 = VERTEX_POINT ( 'NONE', #2294 ) ;
#3407 = ORIENTED_EDGE ( 'NONE', *, *, #1371, .F. ) ;
#3408 = CIRCLE ( 'NONE', #7958, 0.4692913385826771866 ) ;
#3409 = DIRECTION ( 'NONE',  ( 0.7071067811865470176, 0.7071067811865480168, 0.000000000000000000 ) ) ;
#3410 = LINE ( 'NONE', #20666, #1187 ) ;
#3411 = VERTEX_POINT ( 'NONE', #26035 ) ;
#3412 = DIRECTION ( 'NONE',  ( -0.000000000000000000, 1.000000000000000000, -0.000000000000000000 ) ) ;
#3413 = ORIENTED_EDGE ( 'NONE', *, *, #20354, .F. ) ;
#3414 = CARTESIAN_POINT ( 'NONE',  ( 0.4010740433761567081, 4.911740434416970370E-17, -0.2480314960629921295 ) ) ;
#3415 = EDGE_LOOP ( 'NONE', ( #27420, #16968 ) ) ;
#3416 = CARTESIAN_POINT ( 'NONE',  ( 0.2006393256663384084, 0.4069519308876483610, -1.934055118110236338 ) ) ;
#3417 = DIRECTION ( 'NONE',  ( 0.000000000000000000, 0.000000000000000000, 1.000000000000000000 ) ) ;
#3418 = CARTESIAN_POINT ( 'NONE',  ( 0.5383572925355708527, -0.3100567972184350429, 0.2574803149606298969 ) ) ;
#3419 = CARTESIAN_POINT ( 'NONE',  ( 0.03190927504541822557, 0.3133984839257918931, -3.179301372150324045 ) ) ;
#3420 = DIRECTION ( 'NONE',  ( -1.000000000000000000, 0.000000000000000000, 0.000000000000000000 ) ) ;
#3421 = PLANE ( 'NONE',  #6401 ) ;
#3422 = EDGE_CURVE ( 'NONE', #18692, #19022, #26099, .T. ) ;
#3423 = ORIENTED_EDGE ( 'NONE', *, *, #2871, .F. ) ;
#3424 = CARTESIAN_POINT ( 'NONE',  ( 0.000000000000000000, 0.000000000000000000, -0.2342519685039370358 ) ) ;
#3425 = DIRECTION ( 'NONE',  ( -1.000000000000000000, 0.000000000000000000, 0.000000000000000000 ) ) ;
#3426 = PRODUCT_DEFINITION_FORMATION_WITH_SPECIFIED_SOURCE ( 'ANY', '', #16553, .NOT_KNOWN. ) ;
#3427 = DIRECTION ( 'NONE',  ( -0.9790454724845842893, 0.1018208755700882318, 0.1763589297585410332 ) ) ;
#3428 = EDGE_CURVE ( 'NONE', #14935, #24679, #9414, .T. ) ;
#3429 = AXIS2_PLACEMENT_3D ( 'NONE', #25649, #6303, #23547 ) ;
#3430 = CARTESIAN_POINT ( 'NONE',  ( 0.3552036222398872733, -0.04673558830919831431, -3.115157480314960203 ) ) ;
#3431 = PRODUCT_DEFINITION_CONTEXT ( 'detailed design', #3105, 'design' ) ;
#3432 = ORIENTED_EDGE ( 'NONE', *, *, #13391, .T. ) ;
#3433 = CARTESIAN_POINT ( 'NONE',  ( 0.4446020952038907681, 0.02909913904662021419, -1.934055118110236338 ) ) ;
#3434 = AXIS2_PLACEMENT_3D ( 'NONE', #4019, #23665, #25768 ) ;
#3435 = B_SPLINE_CURVE_WITH_KNOTS ( 'NONE', 3,
 ( #456, #17538, #19667, #13564, #9175, #13297, #26152, #6808 ),
 .UNSPECIFIED., .F., .F.,
 ( 4, 2, 2, 4 ),
 ( 0.5000000000000000000, 0.7500000000000002220, 0.8750000000000000000, 1.000000000000000000 ),
 .UNSPECIFIED. ) ;
#3436 = EDGE_LOOP ( 'NONE', ( #21121, #8303 ) ) ;
#3437 = ORIENTED_EDGE ( 'NONE', *, *, #14859, .F. ) ;
#3438 = CARTESIAN_POINT ( 'NONE',  ( -0.3376790527244098450, -1.075350501301808981, -0.6872880233270275419 ) ) ;
#3439 = DIRECTION ( 'NONE',  ( 1.000000000000000000, 0.000000000000000000, 0.000000000000000000 ) ) ;
#3440 = CARTESIAN_POINT ( 'NONE',  ( -0.5280699926563169333, 0.06957181182499308503, 1.747047244094488194 ) ) ;
#3441 = ORIENTED_EDGE ( 'NONE', *, *, #26709, .T. ) ;
#3442 = CARTESIAN_POINT ( 'NONE',  ( -0.07874015748031489015, 0.000000000000000000, -0.3779527559055118058 ) ) ;
#3443 = ORIENTED_EDGE ( 'NONE', *, *, #13804, .F. ) ;
#3444 = AXIS2_PLACEMENT_3D ( 'NONE', #18198, #13847, #5077 ) ;
#3445 = B_SPLINE_CURVE_WITH_KNOTS ( 'NONE', 3,
 ( #24907, #14048, #16438, #26890, #7255, #9934 ),
 .UNSPECIFIED., .F., .F.,
 ( 4, 2, 4 ),
 ( 0.2291966065698869959, 0.2305109203526899964, 0.2318252341354939960 ),
 .UNSPECIFIED. ) ;
#3446 = CARTESIAN_POINT ( 'NONE',  ( -0.3765118517642104257, -0.02464264302297883638, -3.100567304031763172 ) ) ;
#3447 = MANIFOLD_SOLID_BREP ( 'M6 Thin Hex Nut', #10992 ) ;
#3448 = CARTESIAN_POINT ( 'NONE',  ( 0.7874015748031496509, 0.3205050385779313893, -0.05203301786850960536 ) ) ;
#3449 = PRODUCT ( 'Shaft Seal 15x26x7', 'Shaft Seal 15x26x7', '', ( #15092 ) ) ;
#3450 = CARTESIAN_POINT ( 'NONE',  ( -0.2256712916308122319, 2.828271352002458705E-17, -4.330708661396418080 ) ) ;
#3451 = ORIENTED_EDGE ( 'NONE', *, *, #25299, .T. ) ;
#3452 = EDGE_CURVE ( 'NONE', #10641, #13674, #10781, .T. ) ;
#3453 = AXIS2_PLACEMENT_3D ( 'NONE', #15418, #24005, #19767 ) ;
#3454 = CIRCLE ( 'NONE', #17881, 0.5007874015748031704 ) ;
#3455 = CARTESIAN_POINT ( 'NONE',  ( -0.8031496062992127261, 9.835745945907876618E-17, 0.4488188976377953110 ) ) ;
#3456 = ORIENTED_EDGE ( 'NONE', *, *, #12071, .T. ) ;
#3457 = DIRECTION ( 'NONE',  ( 5.737213000000000442E-16, -1.000000000000000000, 0.000000000000000000 ) ) ;
#3458 = CARTESIAN_POINT ( 'NONE',  ( -0.07874015748031495954, 0.000000000000000000, 0.000000000000000000 ) ) ;
#3459 = EDGE_LOOP ( 'NONE', ( #14828, #18126 ) ) ;
#3460 = CARTESIAN_POINT ( 'NONE',  ( 0.2228126397719810137, -0.3858397471888643793, -1.934055118110236338 ) ) ;
#3461 = ORIENTED_EDGE ( 'NONE', *, *, #9918, .F. ) ;
#3462 = VERTEX_POINT ( 'NONE', #26169 ) ;
#3463 = DIRECTION ( 'NONE',  ( 0.000000000000000000, -1.000000000000000000, 0.000000000000000000 ) ) ;
#3464 = EDGE_CURVE ( 'NONE', #14369, #27683, #17089, .T. ) ;
#3465 = CARTESIAN_POINT ( 'NONE',  ( 0.3213305936751376102, 0.1584254766472200371, -3.115157480314960647 ) ) ;
#3466 = DIRECTION ( 'NONE',  ( 1.000000000000000000, 0.000000000000000000, 0.000000000000000000 ) ) ;
#3467 = CARTESIAN_POINT ( 'NONE',  ( -0.6889763779527560139, 0.000000000000000000, -0.2618110236220472231 ) ) ;
#3468 = DIRECTION ( 'NONE',  ( -0.000000000000000000, -0.000000000000000000, 1.000000000000000000 ) ) ;
#3469 = ADVANCED_FACE ( 'NONE', ( #17679 ), #10297, .F. ) ;
#3470 = DIRECTION ( 'NONE',  ( 0.000000000000000000, 0.000000000000000000, -1.000000000000000000 ) ) ;
#3471 = CARTESIAN_POINT ( 'NONE',  ( 1.446433227339386678E-17, 0.4724409448818898127, -1.574803149606299524 ) ) ;
#3472 = CARTESIAN_POINT ( 'NONE',  ( -2.685748425196850164E-17, 0.000000000000000000, -3.745078740157480546 ) ) ;
#3473 = ( GEOMETRIC_REPRESENTATION_CONTEXT ( 3 ) GLOBAL_UNCERTAINTY_ASSIGNED_CONTEXT ( ( #1750 ) ) GLOBAL_UNIT_ASSIGNED_CONTEXT ( ( #8720, #22365, #26090 ) ) REPRESENTATION_CONTEXT ( 'NONE', 'WORKASPACE' ) ) ;
#3474 = CARTESIAN_POINT ( 'NONE',  ( 0.2676050456844303871, -0.2056553984168022209, 1.973425196850394192 ) ) ;
#3475 = CARTESIAN_POINT ( 'NONE',  ( 0.0006737210091392942029, 0.6438792636745043207, 0.2359405056220706121 ) ) ;
#3476 = AXIS2_PLACEMENT_3D ( 'NONE', #15362, #6861, #260 ) ;
#3477 = ORIENTED_EDGE ( 'NONE', *, *, #8160, .T. ) ;
#3478 = DIRECTION ( 'NONE',  ( 0.000000000000000000, -1.000000000000000000, 0.000000000000000000 ) ) ;
#3479 = DIRECTION ( 'NONE',  ( -0.000000000000000000, -1.000000000000000000, -0.000000000000000000 ) ) ;
#3480 = DIRECTION ( 'NONE',  ( 0.000000000000000000, -0.9659258263664941557, -0.2588190448135637145 ) ) ;
#3481 = CARTESIAN_POINT ( 'NONE',  ( 0.5394643376411901725, -0.1051622988770984091, 0.2362204724409454060 ) ) ;
#3482 = CARTESIAN_POINT ( 'NONE',  ( 0.5118110236220472231, 0.000000000000000000, 1.747047244094488194 ) ) ;
#3483 = APPLICATION_CONTEXT ( 'automotive_design' ) ;
#3484 = CARTESIAN_POINT ( 'NONE',  ( -0.03349795313264326141, 0.5118110236220472231, 1.747047244094488194 ) ) ;
#3485 = ORIENTED_EDGE ( 'NONE', *, *, #3359, .T. ) ;
#3486 = CARTESIAN_POINT ( 'NONE',  ( -0.3574975638436101444, 0.02339816079122976691, -3.115157480314960647 ) ) ;
#3487 = EDGE_LOOP ( 'NONE', ( #23107, #786 ) ) ;
#3488 = CARTESIAN_POINT ( 'NONE',  ( -0.8267716535433071723, 1.012503259137575512E-16, 0.02362204724409448786 ) ) ;
#3489 = CARTESIAN_POINT ( 'NONE',  ( -0.4446020952038907681, 0.000000000000000000, -1.934055118110236338 ) ) ;
#3490 = CARTESIAN_POINT ( 'NONE',  ( 0.1512834625133127053, -0.4870552862737996813, 0.04694520391073944698 ) ) ;
#3491 = CYLINDRICAL_SURFACE ( 'NONE', #18443, 0.5531496062992126150 ) ;
#3492 = ORIENTED_EDGE ( 'NONE', *, *, #27512, .T. ) ;
#3493 = CARTESIAN_POINT ( 'NONE',  ( -0.06441834428466612639, 0.4889536969035325753, -1.569881889763779625 ) ) ;
#3494 = EDGE_CURVE ( 'NONE', #23576, #24515, #4893, .T. ) ;
#3495 = DIRECTION ( 'NONE',  ( -1.000000000000000000, 0.000000000000000000, 0.000000000000000000 ) ) ;
#3496 = ( GEOMETRIC_REPRESENTATION_CONTEXT ( 3 ) GLOBAL_UNCERTAINTY_ASSIGNED_CONTEXT ( ( #12494 ) ) GLOBAL_UNIT_ASSIGNED_CONTEXT ( ( #904, #22221, #26589 ) ) REPRESENTATION_CONTEXT ( 'NONE', 'WORKASPACE' ) ) ;
#3497 = VECTOR ( 'NONE', #20294, 39.37007874015748143 ) ;
#3498 = ORIENTED_EDGE ( 'NONE', *, *, #235, .T. ) ;
#3499 = VERTEX_POINT ( 'NONE', #19809 ) ;
#3500 = EDGE_CURVE ( 'NONE', #23791, #1325, #26299, .T. ) ;
#3501 = DIRECTION ( 'NONE',  ( -1.000000000000000000, 0.000000000000000000, 0.000000000000000000 ) ) ;
#3502 = CARTESIAN_POINT ( 'NONE',  ( 0.000000000000000000, 0.000000000000000000, 0.2574803149606298969 ) ) ;
#3503 = CARTESIAN_POINT ( 'NONE',  ( 0.5376957092749645728, -0.3112026930392428614, 0.09685039370078740717 ) ) ;
#3504 = EDGE_CURVE ( 'NONE', #23082, #16707, #15586, .T. ) ;
#3505 = CIRCLE ( 'NONE', #23851, 0.1476377952755905387 ) ;
#3506 = EDGE_CURVE ( 'NONE', #18857, #16353, #27007, .T. ) ;
#3507 = DIRECTION ( 'NONE',  ( 1.000000000000000000, 0.000000000000000000, 0.000000000000000000 ) ) ;
#3508 = CARTESIAN_POINT ( 'NONE',  ( 0.01230314960629921330, 0.000000000000000000, 0.000000000000000000 ) ) ;
#3509 = CARTESIAN_POINT ( 'NONE',  ( -0.6091215340374328546, -0.1684002209738235112, 0.2251732882052777107 ) ) ;
#3510 = AXIS2_PLACEMENT_3D ( 'NONE', #1997, #26146, #7168 ) ;
#3511 = CARTESIAN_POINT ( 'NONE',  ( 0.2965233727166233790, 0.3524965443697388734, 0.1771653543307087630 ) ) ;
#3512 = AXIS2_PLACEMENT_3D ( 'NONE', #10785, #15718, #19545 ) ;
#3513 = DIRECTION ( 'NONE',  ( -0.000000000000000000, -1.000000000000000000, -0.000000000000000000 ) ) ;
#3514 = CARTESIAN_POINT ( 'NONE',  ( -0.4157391792961063204, 0.3323952789219086768, 0.1322834645669291320 ) ) ;
#3515 = VERTEX_POINT ( 'NONE', #4291 ) ;
#3516 = VECTOR ( 'NONE', #2253, 39.37007874015748143 ) ;
#3517 = ORIENTED_EDGE ( 'NONE', *, *, #3621, .T. ) ;
#3518 = CARTESIAN_POINT ( 'NONE',  ( -3.616083068348483797E-17, -0.2952755905511810774, 0.01181102362204724393 ) ) ;
#3519 = ORIENTED_EDGE ( 'NONE', *, *, #26581, .T. ) ;
#3520 = DIRECTION ( 'NONE',  ( 0.000000000000000000, 0.000000000000000000, 1.000000000000000000 ) ) ;
#3521 = CARTESIAN_POINT ( 'NONE',  ( -0.09139240964747702423, 0.07874015748031500117, -1.981023540891279271E-18 ) ) ;
#3522 = CARTESIAN_POINT ( 'NONE',  ( -0.04956879678465797578, 0.1968503937007203553, -3.634230943941200831 ) ) ;
#3523 = EDGE_LOOP ( 'NONE', ( #19442, #21347, #13019, #12962 ) ) ;
#3524 = EDGE_CURVE ( 'NONE', #5922, #27503, #14854, .T. ) ;
#3525 = DIRECTION ( 'NONE',  ( -0.000000000000000000, -1.000000000000000000, -0.000000000000000000 ) ) ;
#3526 = VERTEX_POINT ( 'NONE', #12203 ) ;
#3527 = CIRCLE ( 'NONE', #12131, 0.07874015748031489015 ) ;
#3528 = EDGE_CURVE ( 'NONE', #21046, #23841, #15047, .T. ) ;
#3529 = CARTESIAN_POINT ( 'NONE',  ( -0.2195865873856400752, -0.6052790189082013494, 0.2359405056219452124 ) ) ;
#3530 = AXIS2_PLACEMENT_3D ( 'NONE', #9173, #7487, #22603 ) ;
#3531 = DIRECTION ( 'NONE',  ( 0.000000000000000000, 0.000000000000000000, 1.000000000000000000 ) ) ;
#3532 = CARTESIAN_POINT ( 'NONE',  ( -0.0003954787107570692452, 0.5007872847596378518, 0.09684874903502814492 ) ) ;
#3533 = ORIENTED_EDGE ( 'NONE', *, *, #10907, .T. ) ;
#3534 = CARTESIAN_POINT ( 'NONE',  ( -2.185478346456693112E-16, 0.000000000000000000, 0.000000000000000000 ) ) ;
#3535 = CARTESIAN_POINT ( 'NONE',  ( 0.4599954779394911930, -0.2268956277333457894, -1.550196850393700920 ) ) ;
#3536 = EDGE_LOOP ( 'NONE', ( #2757, #18553 ) ) ;
#3537 = VECTOR ( 'NONE', #15870, 39.37007874015748143 ) ;
#3538 = CARTESIAN_POINT ( 'NONE',  ( -0.5118110236220763110, -0.03349795313034512750, -1.550196850393700920 ) ) ;
#3539 = CARTESIAN_POINT ( 'NONE',  ( 0.4407612517155324872, 0.3387265385688508768, 0.9202755905511812440 ) ) ;
#3540 = CARTESIAN_POINT ( 'NONE',  ( -0.5511811023622048555, 0.03607471876259065596, 0.9399606299212598381 ) ) ;
#3541 = CARTESIAN_POINT ( 'NONE',  ( -0.1230388948648306058, -0.3365682031891569781, 0.1805249803386037022 ) ) ;
#3542 = VERTEX_POINT ( 'NONE', #27613 ) ;
#3543 = DIRECTION ( 'NONE',  ( 0.000000000000000000, 0.000000000000000000, -1.000000000000000000 ) ) ;
#3544 = LINE ( 'NONE', #5262, #78 ) ;
#3545 = CONICAL_SURFACE ( 'NONE', #3099, 0.3224687058348476576, 0.8056700744428512140 ) ;
#3546 = AXIS2_PLACEMENT_3D ( 'NONE', #17760, #9267, #5182 ) ;
#3547 = CARTESIAN_POINT ( 'NONE',  ( 0.5376957092749645728, -0.3112026930392428614, 0.09685039370078740717 ) ) ;
#3548 = ORIENTED_EDGE ( 'NONE', *, *, #19521, .F. ) ;
#3549 = ORIENTED_EDGE ( 'NONE', *, *, #9458, .F. ) ;
#3550 = DIRECTION ( 'NONE',  ( 0.000000000000000000, 1.000000000000000000, 0.000000000000000000 ) ) ;
#3552 = CARTESIAN_POINT ( 'NONE',  ( 8.741913385826771462E-17, -4.420669291338583154E-18, 0.000000000000000000 ) ) ;
#3551 = VECTOR ( 'NONE', #16165, 39.37007874015748143 ) ;
#3553 = CARTESIAN_POINT ( 'NONE',  ( 0.000000000000000000, 0.000000000000000000, -0.01377952755905511792 ) ) ;
#3554 = CARTESIAN_POINT ( 'NONE',  ( 0.000000000000000000, 0.4724409448818896462, 0.000000000000000000 ) ) ;
#3555 = VERTEX_POINT ( 'NONE', #1610 ) ;
#3556 = CARTESIAN_POINT ( 'NONE',  ( -0.02559055118110236185, -0.6299212598425196763, 7.714310545810098438E-17 ) ) ;
#3557 = ORIENTED_EDGE ( 'NONE', *, *, #5572, .T. ) ;
#3558 = FACE_OUTER_BOUND ( 'NONE', #10210, .T. ) ;
#3559 = DIRECTION ( 'NONE',  ( -0.4999999999999996114, 0.8660254037844389297, 0.000000000000000000 ) ) ;
#3560 = CARTESIAN_POINT ( 'NONE',  ( 0.3015072509068775219, 0.3596217111730925509, 0.07637549214372835182 ) ) ;
#3561 = DIRECTION ( 'NONE',  ( -1.000000000000000000, 0.000000000000000000, 0.000000000000000000 ) ) ;
#3562 = LINE ( 'NONE', #14482, #21706 ) ;
#3563 = VERTEX_POINT ( 'NONE', #18687 ) ;
#3564 = CIRCLE ( 'NONE', #22995, 0.1299212598425196763 ) ;
#3565 = CARTESIAN_POINT ( 'NONE',  ( 0.000000000000000000, 0.000000000000000000, -0.2342519685039370358 ) ) ;
#3566 = CIRCLE ( 'NONE', #1794, 0.5322834645669292097 ) ;
#3567 = CARTESIAN_POINT ( 'NONE',  ( 0.000000000000000000, 0.000000000000000000, 0.03818897637795275884 ) ) ;
#3568 = CARTESIAN_POINT ( 'NONE',  ( -0.3552078253616823833, -0.04672900338023027594, -3.115157480314959759 ) ) ;
#3569 = CARTESIAN_POINT ( 'NONE',  ( -0.0006479495459704965547, 0.5014297259264257622, 0.1643955689169025458 ) ) ;
#3570 = AXIS2_PLACEMENT_3D ( 'NONE', #23741, #14865, #12984 ) ;
#3571 = ORIENTED_EDGE ( 'NONE', *, *, #27347, .F. ) ;
#3572 = CARTESIAN_POINT ( 'NONE',  ( 0.2712027394948776093, -0.3535065162672919037, -1.934055118110236338 ) ) ;
#3573 = ADVANCED_FACE ( 'NONE', ( #1891 ), #18981, .F. ) ;
#3574 = ADVANCED_FACE ( 'NONE', ( #8255 ), #831, .T. ) ;
#3575 = SHAPE_REPRESENTATION ( 'Rear Bearing Cover', ( #11588 ), #19278 ) ;
#3576 = ADVANCED_FACE ( 'NONE', ( #23240 ), #25659, .F. ) ;
#3577 = VERTEX_POINT ( 'NONE', #14915 ) ;
#3578 = ORIENTED_EDGE ( 'NONE', *, *, #25897, .F. ) ;
#3579 = VERTEX_POINT ( 'NONE', #17015 ) ;
#3580 = ORIENTED_EDGE ( 'NONE', *, *, #17104, .T. ) ;
#3581 = PRODUCT_RELATED_PRODUCT_CATEGORY ( 'part', '', ( #163 ) ) ;
#3582 = CARTESIAN_POINT ( 'NONE',  ( 0.5375739373539409893, 0.4296723508511047229, 0.1322834645669291320 ) ) ;
#3583 = CARTESIAN_POINT ( 'NONE',  ( 0.000000000000000000, 0.000000000000000000, 0.2362204724409449064 ) ) ;
#3584 = CARTESIAN_POINT ( 'NONE',  ( 0.1378076643338917162, 0.5144970376936037759, 1.747047244094488194 ) ) ;
#3585 = EDGE_CURVE ( 'NONE', #10706, #10366, #10435, .T. ) ;
#3586 = ORIENTED_EDGE ( 'NONE', *, *, #19012, .T. ) ;
#3587 = DIRECTION ( 'NONE',  ( 0.000000000000000000, -0.8660254037844385966, -0.4999999999999998335 ) ) ;
#3588 = CIRCLE ( 'NONE', #23495, 0.6299212598425196763 ) ;
#3589 = ORIENTED_EDGE ( 'NONE', *, *, #2917, .T. ) ;
#3590 = VECTOR ( 'NONE', #6075, 39.37007874015748143 ) ;
#3591 = CARTESIAN_POINT ( 'NONE',  ( 0.3644697409450263215, 0.09762295995069791843, -3.100567304031765836 ) ) ;
#3592 = ADVANCED_FACE ( 'NONE', ( #2568 ), #20689, .T. ) ;
#3593 = EDGE_CURVE ( 'NONE', #15868, #17285, #8064, .T. ) ;
#3594 = PLANE ( 'NONE',  #4329 ) ;
#3595 = CARTESIAN_POINT ( 'NONE',  ( 0.09590060490395689585, -0.1136516277932334562, 0.1968503937007874127 ) ) ;
#3596 = CARTESIAN_POINT ( 'NONE',  ( -0.2669480828848088128, -0.2341512108694275007, 1.953740157480315043 ) ) ;
#3597 = ORIENTED_EDGE ( 'NONE', *, *, #10686, .F. ) ;
#3598 = CARTESIAN_POINT ( 'NONE',  ( -0.4958319195689224190, -0.3652762862495049223, -0.3220933753858993831 ) ) ;
#3600 = CARTESIAN_POINT ( 'NONE',  ( -0.5526079293737016229, 0.1480156394741962422, 0.9399606299212598381 ) ) ;
#3599 = CARTESIAN_POINT ( 'NONE',  ( -0.3765118517642104257, 2.305470170520414967E-17, -3.100567304031763172 ) ) ;
#3601 = CARTESIAN_POINT ( 'NONE',  ( 0.000000000000000000, 0.000000000000000000, 0.01181102362204724393 ) ) ;
#3602 = ORIENTED_EDGE ( 'NONE', *, *, #13300, .F. ) ;
#3603 = ORIENTED_EDGE ( 'NONE', *, *, #1922, .F. ) ;
#3604 = DIRECTION ( 'NONE',  ( 0.000000000000000000, 0.000000000000000000, -1.000000000000000000 ) ) ;
#3605 = LINE ( 'NONE', #16340, #11324 ) ;
#3606 = ADVANCED_BREP_SHAPE_REPRESENTATION ( 'Index Plate', ( #2707, #11588 ), #8455 ) ;
#3607 = CARTESIAN_POINT ( 'NONE',  ( 0.2842490391651530390, 0.2180698645301770711, -3.115157480314960647 ) ) ;
#3608 = CARTESIAN_POINT ( 'NONE',  ( 0.1442704874421230632, -0.5368353335967093187, 0.9202755905511807999 ) ) ;
#3609 = CARTESIAN_POINT ( 'NONE',  ( 0.000000000000000000, 0.000000000000000000, 0.07637795275590551769 ) ) ;
#3610 = CARTESIAN_POINT ( 'NONE',  ( -0.05118110236220472370, 0.7539370078740157410, 0.000000000000000000 ) ) ;
#3611 = DIRECTION ( 'NONE',  ( 0.000000000000000000, 1.000000000000000000, 0.000000000000000000 ) ) ;
#3612 = AXIS2_PLACEMENT_3D ( 'NONE', #17620, #13651, #26234 ) ;
#3613 = B_SPLINE_CURVE_WITH_KNOTS ( 'NONE', 3,
 ( #11138, #9009, #19895, #17630, #26250, #6910, #20029, #681 ),
 .UNSPECIFIED., .F., .F.,
 ( 4, 2, 2, 4 ),
 ( 0.001552469560294957029, 0.001994063167382608553, 0.002435656774470260078, 0.003318843988645562692 ),
 .UNSPECIFIED. ) ;
#3614 = ORIENTED_EDGE ( 'NONE', *, *, #8978, .T. ) ;
#3615 = LINE ( 'NONE', #12246, #4669 ) ;
#3616 = ADVANCED_FACE ( 'NONE', ( #26434 ), #7101, .T. ) ;
#3617 = CARTESIAN_POINT ( 'NONE',  ( -0.5382469622846938195, -0.3102483656526051625, 0.09684874924366436433 ) ) ;
#3618 = CIRCLE ( 'NONE', #21691, 0.3937007874015748254 ) ;
#3619 = DIRECTION ( 'NONE',  ( 0.000000000000000000, 0.000000000000000000, -1.000000000000000000 ) ) ;
#3620 = DIRECTION ( 'NONE',  ( 0.000000000000000000, 0.000000000000000000, 1.000000000000000000 ) ) ;
#3621 = EDGE_CURVE ( 'NONE', #16090, #10521, #23858, .T. ) ;
#3622 = DIRECTION ( 'NONE',  ( 0.000000000000000000, 0.000000000000000000, -1.000000000000000000 ) ) ;
#3623 = SURFACE_SIDE_STYLE ('',( #3917 ) ) ;
#3624 = APPLICATION_PROTOCOL_DEFINITION ( 'draft international standard', 'automotive_design', 1998, #19550 ) ;
#3625 = DIMENSIONAL_EXPONENTS ( 1.000000000000000000, 0.000000000000000000, 0.000000000000000000, 0.000000000000000000, 0.000000000000000000, 0.000000000000000000, 0.000000000000000000 ) ;
#3626 = EDGE_CURVE ( 'NONE', #27013, #12986, #15457, .T. ) ;
#3627 = CARTESIAN_POINT ( 'NONE',  ( 0.4441657790107856330, -0.2564944395515579845, 1.766732283464566899 ) ) ;
#3628 = ORIENTED_EDGE ( 'NONE', *, *, #22714, .F. ) ;
#3629 = PLANE ( 'NONE',  #1604 ) ;
#3630 = VERTEX_POINT ( 'NONE', #2171 ) ;
#3631 = EDGE_CURVE ( 'NONE', #240, #14102, #4294, .T. ) ;
#3632 = CARTESIAN_POINT ( 'NONE',  ( 0.000000000000000000, 0.000000000000000000, -0.2480314960629921295 ) ) ;
#3633 = CARTESIAN_POINT ( 'NONE',  ( -0.1968503937007874127, -0.07874015748031495954, 0.04546065111729338803 ) ) ;
#3634 = CARTESIAN_POINT ( 'NONE',  ( -0.5905511811023621549, 0.000000000000000000, 0.000000000000000000 ) ) ;
#3635 = ORIENTED_EDGE ( 'NONE', *, *, #16621, .F. ) ;
#3636 = AXIS2_PLACEMENT_3D ( 'NONE', #19978, #11362, #24351 ) ;
#3637 = CARTESIAN_POINT ( 'NONE',  ( 0.4669911931914377257, 0.1585706980422264545, -1.550196850393700920 ) ) ;
#3638 = ORIENTED_EDGE ( 'NONE', *, *, #20353, .F. ) ;
#3639 = ORIENTED_EDGE ( 'NONE', *, *, #26581, .F. ) ;
#3640 = ORIENTED_EDGE ( 'NONE', *, *, #23073, .T. ) ;
#3641 = EDGE_CURVE ( 'NONE', #23196, #17206, #10923, .T. ) ;
#3642 = ITEM_DEFINED_TRANSFORMATION ( 'NONE', 'NONE', #26018,  #11588 ) ;
#3643 = CARTESIAN_POINT ( 'NONE',  ( 0.0005189969344232283309, 0.3771649972486724733, 0.07637795275590551769 ) ) ;
#3644 = DIRECTION ( 'NONE',  ( 0.000000000000000000, 0.000000000000000000, 1.000000000000000000 ) ) ;
#3645 = CARTESIAN_POINT ( 'NONE',  ( 0.000000000000000000, 0.000000000000000000, -0.4724409448841456749 ) ) ;
#3646 = DIRECTION ( 'NONE',  ( 0.000000000000000000, -1.000000000000000000, 0.000000000000000000 ) ) ;
#3647 = ORIENTED_EDGE ( 'NONE', *, *, #5093, .T. ) ;
#3648 = CARTESIAN_POINT ( 'NONE',  ( 0.1287090038540881498, 0.1704774416898497957, 0.09842519685039405331 ) ) ;
#3649 = APPLICATION_CONTEXT ( 'automotive_design' ) ;
#3650 = UNCERTAINTY_MEASURE_WITH_UNIT (LENGTH_MEASURE( 1.000000000000000082E-05 ), #13265, 'distance_accuracy_value', 'NONE') ;
#3651 = FACE_OUTER_BOUND ( 'NONE', #18681, .T. ) ;
#3652 = CARTESIAN_POINT ( 'NONE',  ( 0.000000000000000000, 0.4232283464566928832, 0.1377952755905511861 ) ) ;
#3653 = CARTESIAN_POINT ( 'NONE',  ( -2.273123186440590970, -0.6468501409757874132, 2.027559055118110187 ) ) ;
#3654 = EDGE_CURVE ( 'NONE', #1673, #2756, #24054, .T. ) ;
#3655 = CARTESIAN_POINT ( 'NONE',  ( -0.5347915442629350702, -0.4325403863649552871, 0.1614721600616167985 ) ) ;
#3656 = CARTESIAN_POINT ( 'NONE',  ( -0.002724751885583818600, 4.306736220472441732E-16, -0.1968503937007877458 ) ) ;
#3657 = DIRECTION ( 'NONE',  ( -0.8571673003991039375, 0.000000000000000000, -0.5150380754143447648 ) ) ;
#3658 = CARTESIAN_POINT ( 'NONE',  ( -0.7874015748031496509, -5.862181872755905604E-06, -1.869015748010449007 ) ) ;
#3659 = EDGE_CURVE ( 'NONE', #8851, #18698, #97, .T. ) ;
#3660 = AXIS2_PLACEMENT_3D ( 'NONE', #26675, #26822, #22446 ) ;
#3661 = AXIS2_PLACEMENT_3D ( 'NONE', #3583, #25070, #5734 ) ;
#3662 = EDGE_LOOP ( 'NONE', ( #25309, #5752, #22752, #9765, #6498, #1916, #18496, #8610 ) ) ;
#3663 = AXIS2_PLACEMENT_3D ( 'NONE', #18497, #5815, #1847 ) ;
#3664 = ORIENTED_EDGE ( 'NONE', *, *, #25024, .T. ) ;
#3665 = DIRECTION ( 'NONE',  ( 0.000000000000000000, 0.000000000000000000, 1.000000000000000000 ) ) ;
#3666 = EDGE_CURVE ( 'NONE', #12544, #11206, #13316, .T. ) ;
#3667 = ORIENTED_EDGE ( 'NONE', *, *, #3806, .F. ) ;
#3668 = CARTESIAN_POINT ( 'NONE',  ( -0.3217486617182078734, 0.3837523410419874659, 0.09684793308443542803 ) ) ;
#3669 = CYLINDRICAL_SURFACE ( 'NONE', #14846, 0.7874015748031496509 ) ;
#3670 = CARTESIAN_POINT ( 'NONE',  ( 0.000000000000000000, 0.000000000000000000, 0.1771653543307086520 ) ) ;
#3671 = ORIENTED_EDGE ( 'NONE', *, *, #6583, .T. ) ;
#3672 = CARTESIAN_POINT ( 'NONE',  ( -1.692913385826771533, 0.07874015748031491790, 0.1181102362204718981 ) ) ;
#3673 = VERTEX_POINT ( 'NONE', #11196 ) ;
#3674 = EDGE_CURVE ( 'NONE', #9013, #16391, #17932, .T. ) ;
#3675 = DIRECTION ( 'NONE',  ( 0.000000000000000000, 0.000000000000000000, 1.000000000000000000 ) ) ;
#3676 = CIRCLE ( 'NONE', #20842, 0.07677362204724411110 ) ;
#3677 = CARTESIAN_POINT ( 'NONE',  ( 0.003937007874015826907, -4.393043307086613241E-18, 0.000000000000000000 ) ) ;
#3678 = DIRECTION ( 'NONE',  ( -1.000000000000000000, 0.000000000000000000, 0.000000000000000000 ) ) ;
#3679 = AXIS2_PLACEMENT_3D ( 'NONE', #19825, #10934, #486 ) ;
#3680 = CYLINDRICAL_SURFACE ( 'NONE', #9596, 0.1181102362204718703 ) ;
#3681 = ORIENTED_EDGE ( 'NONE', *, *, #6118, .F. ) ;
#3682 = CARTESIAN_POINT ( 'NONE',  ( 0.0004447986960614786845, 0.5322833254990984031, 0.1322818204150988386 ) ) ;
#3683 = CARTESIAN_POINT ( 'NONE',  ( 0.2904160862623688666, 0.1677079028045472542, 1.953740157480315043 ) ) ;
#3684 = PLANE ( 'NONE',  #4186 ) ;
#3685 = EDGE_CURVE ( 'NONE', #16564, #8713, #6703, .T. ) ;
#3686 = CARTESIAN_POINT ( 'NONE',  ( 0.1429116519061375268, 0.5335524835332416949, 0.9399606299212598381 ) ) ;
#3687 = FACE_OUTER_BOUND ( 'NONE', #21920, .T. ) ;
#3688 = DIRECTION ( 'NONE',  ( 0.000000000000000000, -1.000000000000000000, 0.000000000000000000 ) ) ;
#3689 = DIRECTION ( 'NONE',  ( -1.000000000000000000, 0.000000000000000000, 0.000000000000000000 ) ) ;
#3690 = EDGE_LOOP ( 'NONE', ( #8728, #7708, #10424, #22 ) ) ;
#3691 = PRODUCT ( 'Front Bearing Cover', 'Front Bearing Cover', '', ( #1657 ) ) ;
#3692 = CARTESIAN_POINT ( 'NONE',  ( 0.000000000000000000, 0.000000000000000000, 0.01181102362204724393 ) ) ;
#3693 = CARTESIAN_POINT ( 'NONE',  ( 0.3454440660767458815, 0.3030032861725153737, -1.928289503579147635 ) ) ;
#3694 = EDGE_CURVE ( 'NONE', #21183, #11904, #22054, .T. ) ;
#3695 = CIRCLE ( 'NONE', #2409, 0.7874015748031496509 ) ;
#3696 = DIRECTION ( 'NONE',  ( 0.000000000000000000, 1.000000000000000000, 0.000000000000000000 ) ) ;
#3697 = AXIS2_PLACEMENT_3D ( 'NONE', #11160, #17904, #22309 ) ;
#3698 = CARTESIAN_POINT ( 'NONE',  ( 0.06947563356181042649, 0.5280876769850310071, 1.747047244094488194 ) ) ;
#3699 = ORIENTED_EDGE ( 'NONE', *, *, #19527, .F. ) ;
#3700 = VECTOR ( 'NONE', #23424, 39.37007874015748143 ) ;
#3701 = B_SPLINE_CURVE_WITH_KNOTS ( 'NONE', 3,
 ( #3743, #12363, #18560, #12507, #5742, #10230, #22971, #27207 ),
 .UNSPECIFIED., .F., .F.,
 ( 4, 2, 2, 4 ),
 ( 0.000000000000000000, 0.1249999999999998890, 0.2499999999999997780, 0.5000000000000000000 ),
 .UNSPECIFIED. ) ;
#3702 = ( BOUNDED_CURVE ( )  B_SPLINE_CURVE ( 2, ( #7732, #26643, #22844 ),
 .UNSPECIFIED., .F., .T. ) 
 B_SPLINE_CURVE_WITH_KNOTS ( ( 3, 3 ),
 ( 0.000000000000000000, 0.2336872276155829986 ),
 .UNSPECIFIED. ) 
 CURVE ( )  GEOMETRIC_REPRESENTATION_ITEM ( )  RATIONAL_B_SPLINE_CURVE ( ( 1.000000000000000000, 1.154700538379251906, 1.000000000000000000 ) ) 
 REPRESENTATION_ITEM ( '' )  ) ;
#3703 = ORIENTED_EDGE ( 'NONE', *, *, #12278, .T. ) ;
#3704 = CARTESIAN_POINT ( 'NONE',  ( -0.7086614173228346081, 0.000000000000000000, 2.145669291338582862 ) ) ;
#3705 = CARTESIAN_POINT ( 'NONE',  ( 0.000000000000000000, 0.000000000000000000, 0.07637795275590551769 ) ) ;
#3706 = CARTESIAN_POINT ( 'NONE',  ( -0.3511566718596346171, -0.4004902621171045340, 1.747047244094487528 ) ) ;
#3707 = ORIENTED_EDGE ( 'NONE', *, *, #4905, .F. ) ;
#3708 = CARTESIAN_POINT ( 'NONE',  ( -0.0007683673430013719316, 0.7042519390026829029, 0.1443310008634866026 ) ) ;
#3709 = VERTEX_POINT ( 'NONE', #17286 ) ;
#3710 = EDGE_CURVE ( 'NONE', #14499, #7850, #8799, .T. ) ;
#3711 = CARTESIAN_POINT ( 'NONE',  ( -0.6867658503580778007, -0.1559616964373211900, 0.1443310008614889506 ) ) ;
#3712 = LINE ( 'NONE', #25184, #26502 ) ;
#3713 = DIRECTION ( 'NONE',  ( 1.000000000000000000, 0.000000000000000000, 0.000000000000000000 ) ) ;
#3714 = CARTESIAN_POINT ( 'NONE',  ( -0.5616993144963264850, -0.5770964849842729061, -0.9615141454532954990 ) ) ;
#3715 = DIRECTION ( 'NONE',  ( 0.000000000000000000, 1.000000000000000000, 0.000000000000000000 ) ) ;
#3716 = FACE_OUTER_BOUND ( 'NONE', #16941, .T. ) ;
#3717 = FACE_OUTER_BOUND ( 'NONE', #1381, .T. ) ;
#3718 = ORIENTED_EDGE ( 'NONE', *, *, #6749, .F. ) ;
#3719 = AXIS2_PLACEMENT_3D ( 'NONE', #15864, #10941, #19566 ) ;
#3720 = CARTESIAN_POINT ( 'NONE',  ( 0.000000000000000000, 0.000000000000000000, 0.3401574803149606252 ) ) ;
#3721 = CARTESIAN_POINT ( 'NONE',  ( 0.1516263115863346334, 0.4909405214979283838, -0.05579628926458630317 ) ) ;
#3722 = CIRCLE ( 'NONE', #22210, 0.6299212598425196763 ) ;
#3723 = CARTESIAN_POINT ( 'NONE',  ( -0.1968503937007874127, -5.802129921259842692E-18, 0.000000000000000000 ) ) ;
#3724 = AXIS2_PLACEMENT_3D ( 'NONE', #6641, #430, #17889 ) ;
#3725 = CARTESIAN_POINT ( 'NONE',  ( 0.06441834428466665374, -0.4889536969035324088, -1.569881889763779625 ) ) ;
#3726 = VERTEX_POINT ( 'NONE', #24193 ) ;
#3727 = CARTESIAN_POINT ( 'NONE',  ( 0.1432577568504609655, -0.4218945342797526532, -1.934055118110236338 ) ) ;
#3728 = CONICAL_SURFACE ( 'NONE', #24035, 0.8214970631411201429, 0.2617993875000020898 ) ;
#3729 = EDGE_CURVE ( 'NONE', #7673, #3938, #13479, .T. ) ;
#3730 = VERTEX_POINT ( 'NONE', #20649 ) ;
#3731 = ORIENTED_EDGE ( 'NONE', *, *, #16393, .T. ) ;
#3732 = ORIENTED_EDGE ( 'NONE', *, *, #9757, .T. ) ;
#3733 = CARTESIAN_POINT ( 'NONE',  ( -0.5935113537020059171, -0.1411927790378836589, -0.2484461867309594729 ) ) ;
#3734 = CARTESIAN_POINT ( 'NONE',  ( -1.197070535079588716, 0.07874015748031491790, -1.197070535079588716 ) ) ;
#3735 = CARTESIAN_POINT ( 'NONE',  ( -0.1378076643338909391, 0.5144970376935737999, 1.747047244094488194 ) ) ;
#3736 = ORIENTED_EDGE ( 'NONE', *, *, #298, .F. ) ;
#3737 = CARTESIAN_POINT ( 'NONE',  ( 0.000000000000000000, 0.000000000000000000, 0.04842519685039370358 ) ) ;
#3738 = CIRCLE ( 'NONE', #17721, 0.7500000000000001110 ) ;
#3739 = ORIENTED_EDGE ( 'NONE', *, *, #25748, .T. ) ;
#3740 = AXIS2_PLACEMENT_3D ( 'NONE', #25412, #21969, #10955 ) ;
#3741 = CARTESIAN_POINT ( 'NONE',  ( -0.2488091035917020799, -0.2836590635674518524, -3.100567304031764948 ) ) ;
#3742 = EDGE_CURVE ( 'NONE', #12816, #21648, #26115, .T. ) ;
#3743 = CARTESIAN_POINT ( 'NONE',  ( 0.2303471512294322787, -0.4798602677570401598, 0.1322834645669291320 ) ) ;
#3744 = CARTESIAN_POINT ( 'NONE',  ( -0.02319089060378104472, -0.3543307086614173596, 1.953740157480315043 ) ) ;
#3745 = ORIENTED_EDGE ( 'NONE', *, *, #10571, .T. ) ;
#3746 = EDGE_LOOP ( 'NONE', ( #23859, #6534 ) ) ;
#3747 = AXIS2_PLACEMENT_3D ( 'NONE', #13845, #13696, #27128 ) ;
#3748 = CARTESIAN_POINT ( 'NONE',  ( -0.5738238537687410101, -0.1850264159751985327, -0.2573737795900459813 ) ) ;
#3750 = CARTESIAN_POINT ( 'NONE',  ( 0.5335524835332418059, -0.1429116519061131296, 0.9399606299212598381 ) ) ;
#3749 = CARTESIAN_POINT ( 'NONE',  ( 0.000000000000000000, 0.5905511811023621549, 0.000000000000000000 ) ) ;
#3751 = ORIENTED_EDGE ( 'NONE', *, *, #2987, .T. ) ;
#3752 = VERTEX_POINT ( 'NONE', #11747 ) ;
#3753 = DIRECTION ( 'NONE',  ( 0.000000000000000000, 1.000000000000000000, 0.000000000000000000 ) ) ;
#3754 = DIRECTION ( 'NONE',  ( 0.000000000000000000, 0.000000000000000000, 1.000000000000000000 ) ) ;
#3755 = EDGE_CURVE ( 'NONE', #762, #6801, #12034, .T. ) ;
#3756 = CARTESIAN_POINT ( 'NONE',  ( 0.1151913129404419367, -0.3392387706403586223, -3.115157480314960647 ) ) ;
#3757 = DIRECTION ( 'NONE',  ( 1.000000000000000000, 0.000000000000000000, 0.000000000000000000 ) ) ;
#3758 = CARTESIAN_POINT ( 'NONE',  ( 0.000000000000000000, 0.000000000000000000, 1.914370078775489148 ) ) ;
#3759 = CARTESIAN_POINT ( 'NONE',  ( 0.3543307086367249448, 0.000000000000000000, -2.322834645648386154 ) ) ;
#3760 = CIRCLE ( 'NONE', #2869, 0.01968503937007872254 ) ;
#3761 = ( BOUNDED_CURVE ( )  B_SPLINE_CURVE ( 2, ( #8910, #12735, #11040 ),
 .UNSPECIFIED., .F., .T. ) 
 B_SPLINE_CURVE_WITH_KNOTS ( ( 3, 3 ),
 ( 0.000000000000000000, 0.1168436138077912356 ),
 .UNSPECIFIED. ) 
 CURVE ( )  GEOMETRIC_REPRESENTATION_ITEM ( )  RATIONAL_B_SPLINE_CURVE ( ( 1.000000000000000000, 1.077350269189625731, 1.077350269189625953 ) ) 
 REPRESENTATION_ITEM ( '' )  ) ;
#3762 = CARTESIAN_POINT ( 'NONE',  ( 0.000000000000000000, 0.3543307086614172485, 1.377952755905512472 ) ) ;
#3763 = CIRCLE ( 'NONE', #13677, 0.5511811023622047445 ) ;
#3764 = DIRECTION ( 'NONE',  ( 0.5000000000000009992, 0.000000000000000000, 0.8660254037844380415 ) ) ;
#3765 = CARTESIAN_POINT ( 'NONE',  ( -0.3149606299212598381, 3.857155272905049219E-17, -3.745078740157480546 ) ) ;
#3766 = ADVANCED_FACE ( 'NONE', ( #20084 ), #4410, .T. ) ;
#3767 = ORIENTED_EDGE ( 'NONE', *, *, #18502, .T. ) ;
#3768 = FACE_OUTER_BOUND ( 'NONE', #1973, .T. ) ;
#3769 = AXIS2_PLACEMENT_3D ( 'NONE', #26947, #26798, #11404 ) ;
#3770 = FACE_BOUND ( 'NONE', #6327, .T. ) ;
#3771 = FACE_OUTER_BOUND ( 'NONE', #19803, .T. ) ;
#3772 = VERTEX_POINT ( 'NONE', #20861 ) ;
#3773 = VECTOR ( 'NONE', #17359, 39.37007874015748143 ) ;
#3774 = CARTESIAN_POINT ( 'NONE',  ( 0.000000000000000000, 0.000000000000000000, -0.2342519685039370358 ) ) ;
#3775 = DIRECTION ( 'NONE',  ( 0.000000000000000000, 1.000000000000000000, 0.000000000000000000 ) ) ;
#3776 = LINE ( 'NONE', #21010, #14306 ) ;
#3777 = B_SPLINE_CURVE_WITH_KNOTS ( 'NONE', 3,
 ( #20017, #13247, #2508, #8735, #539, #23867, #11127, #4500, #25974, #9130, #24390, #13381, #17624, #6627, #17749, #2365, #4901, #15655, #19623, #293, #24255, #8866, #11398, #672, #17487, #9262, #26107, #6764, #19750, #15397, #23989, #419, #26240, #6898, #7583, #20434, #3322, #9401, #25091, #11675, #11964, #9697, #20584, #16208, #15917 ),
 .UNSPECIFIED., .F., .F.,
 ( 4, 2, 1, 1, 1, 1, 2, 2, 2, 2, 1, 1, 1, 1, 1, 2, 2, 2, 2, 1, 1, 1, 1, 2, 2, 2, 2, 2, 4 ),
 ( 0.000000000000000000, 0.1250000000000077716, 0.1875000000000116018, 0.2187500000000134892, 0.2343750000000144607, 0.2421875000000147937, 0.2460937500000149880, 0.2500000000000151545, 0.3750000000000195399, 0.4375000000000214273, 0.4687500000000222045, 0.4843750000000223710, 0.4921875000000224820, 0.4960937500000226485, 0.4980468750000229816, 0.4990234375000230371, 0.5000000000000230926, 0.6250000000000341949, 0.6875000000000397460, 0.7187500000000424105, 0.7343750000000437428, 0.7421875000000444089, 0.7460937500000445199, 0.7480468750000444089, 0.7500000000000442979, 0.8125000000000331957, 0.8437500000000276446, 0.8750000000000222045, 1.000000000000000000 ),
 .UNSPECIFIED. ) ;
#3778 = CARTESIAN_POINT ( 'NONE',  ( 0.4600326175560556230, -0.2268096725222457644, 1.766732283464566899 ) ) ;
#3779 = EDGE_LOOP ( 'NONE', ( #7984, #23776 ) ) ;
#3780 = ORIENTED_EDGE ( 'NONE', *, *, #20283, .F. ) ;
#3781 = FACE_OUTER_BOUND ( 'NONE', #9605, .T. ) ;
#3782 = VERTEX_POINT ( 'NONE', #27226 ) ;
#3783 = CARTESIAN_POINT ( 'NONE',  ( -0.4233199042353229524, 0.5034331896078060309, 0.1461456498253434766 ) ) ;
#3784 = ( LENGTH_UNIT ( ) NAMED_UNIT ( * ) SI_UNIT ( $, .METRE. ) ) ;
#3785 = CARTESIAN_POINT ( 'NONE',  ( 0.7873254110137047901, 0.3967163408419193127, 0.1736506122128708696 ) ) ;
#3786 = CARTESIAN_POINT ( 'NONE',  ( 0.3339160553493877304, 0.7781263166395089304, -0.8035123328091101635 ) ) ;
#3787 = AXIS2_PLACEMENT_3D ( 'NONE', #6123, #7950, #14758 ) ;
#3788 = CARTESIAN_POINT ( 'NONE',  ( 0.2904160862623631489, 0.1677079028045434517, 1.973425196850393970 ) ) ;
#3789 = ORIENTED_EDGE ( 'NONE', *, *, #4673, .F. ) ;
#3790 = ORIENTED_EDGE ( 'NONE', *, *, #14504, .F. ) ;
#3791 = CARTESIAN_POINT ( 'NONE',  ( 0.3252100150720381722, -0.3707612262533039327, -1.550196850393700920 ) ) ;
#3792 = CARTESIAN_POINT ( 'NONE',  ( -0.3714653163189441387, 0.06532421472592696288, 0.1992150590373740204 ) ) ;
#3793 = ORIENTED_EDGE ( 'NONE', *, *, #8211, .T. ) ;
#3794 = ORIENTED_EDGE ( 'NONE', *, *, #11136, .F. ) ;
#3795 = ORIENTED_EDGE ( 'NONE', *, *, #16719, .T. ) ;
#3796 = CIRCLE ( 'NONE', #15545, 0.4692913385826771866 ) ;
#3797 = EDGE_CURVE ( 'NONE', #16095, #12969, #16768, .T. ) ;
#3798 = CARTESIAN_POINT ( 'NONE',  ( 0.000000000000000000, 0.000000000000000000, 1.707677165389662743 ) ) ;
#3799 = VECTOR ( 'NONE', #27879, 39.37007874015748854 ) ;
#3800 = DIRECTION ( 'NONE',  ( 0.000000000000000000, 0.000000000000000000, 1.000000000000000000 ) ) ;
#3801 = DIRECTION ( 'NONE',  ( 0.000000000000000000, 1.000000000000000000, 0.000000000000000000 ) ) ;
#3802 = CARTESIAN_POINT ( 'NONE',  ( 0.4339912984563291110, -0.2498791196563492356, 0.2574803149606298969 ) ) ;
#3803 = ADVANCED_FACE ( 'NONE', ( #1510 ), #25378, .F. ) ;
#3804 = ORIENTED_EDGE ( 'NONE', *, *, #6435, .F. ) ;
#3805 = CARTESIAN_POINT ( 'NONE',  ( -0.3223547283257516272, 0.3832433309296771617, 0.2574803149606298969 ) ) ;
#3806 = EDGE_CURVE ( 'NONE', #11937, #15780, #19364, .T. ) ;
#3807 = AXIS2_PLACEMENT_3D ( 'NONE', #7636, #3812, #12142 ) ;
#3808 = CARTESIAN_POINT ( 'NONE',  ( 0.1318897637674579792, 0.000000000000000000, 0.9055118110027171596 ) ) ;
#3809 = DIRECTION ( 'NONE',  ( -1.000000000000000000, 0.000000000000000000, 0.000000000000000000 ) ) ;
#3810 = DIRECTION ( 'NONE',  ( 0.9247062791528062320, 0.000000000000000000, -0.3806813592696290938 ) ) ;
#3811 = CARTESIAN_POINT ( 'NONE',  ( -0.4339437742824454047, -0.8141188606247102832, -0.05345644696679699437 ) ) ;
#3812 = DIRECTION ( 'NONE',  ( 0.000000000000000000, 0.8660254037844388186, -0.4999999999999998890 ) ) ;
#3813 = DIRECTION ( 'NONE',  ( 0.000000000000000000, -0.8660254037844385966, 0.4999999999999998335 ) ) ;
#3814 = AXIS2_PLACEMENT_3D ( 'NONE', #9451, #7352, #3091 ) ;
#3815 = CARTESIAN_POINT ( 'NONE',  ( 4.756848988674917118E-17, 0.9055118110236221041, 0.3831516066089791228 ) ) ;
#3816 = ORIENTED_EDGE ( 'NONE', *, *, #7420, .T. ) ;
#3817 = AXIS2_PLACEMENT_3D ( 'NONE', #5847, #27177, #7818 ) ;
#3818 = VERTEX_POINT ( 'NONE', #7877 ) ;
#3819 = VERTEX_POINT ( 'NONE', #5474 ) ;
#3820 = CARTESIAN_POINT ( 'NONE',  ( -0.4954415918535808872, -0.1327036767636090853, -1.550196850393700920 ) ) ;
#3821 = DIRECTION ( 'NONE',  ( -1.147443000000000016E-15, -1.000000000000000000, -0.000000000000000000 ) ) ;
#3822 = CARTESIAN_POINT ( 'NONE',  ( -0.3197948809220744204, -0.6622502000681186329, 0.1960773254378390396 ) ) ;
#3823 = CARTESIAN_POINT ( 'NONE',  ( -0.03607471876262472593, 0.5511811023622047445, 0.9202755905511811330 ) ) ;
#3824 = EDGE_LOOP ( 'NONE', ( #21964, #23743, #16597, #12033 ) ) ;
#3825 = CIRCLE ( 'NONE', #21438, 0.1003937007874015908 ) ;
#3826 = CARTESIAN_POINT ( 'NONE',  ( -0.09139240964747710749, -0.07874015748031500117, -1.188614124534770567E-17 ) ) ;
#3827 = ORIENTED_EDGE ( 'NONE', *, *, #10852, .F. ) ;
#3828 = EDGE_CURVE ( 'NONE', #12846, #24919, #25958, .T. ) ;
#3829 = DIRECTION ( 'NONE',  ( 0.000000000000000000, 0.000000000000000000, 1.000000000000000000 ) ) ;
#3830 = CYLINDRICAL_SURFACE ( 'NONE', #10908, 1.288838582677165556 ) ;
#3831 = CARTESIAN_POINT ( 'NONE',  ( -0.4068940122753434974, -0.3122781343786983355, -1.550196850393701142 ) ) ;
#3832 = ADVANCED_FACE ( 'NONE', ( #16625 ), #8079, .F. ) ;
#3833 = CIRCLE ( 'NONE', #14234, 0.6212598425196850238 ) ;
#3834 = DIRECTION ( 'NONE',  ( -1.000000000000000000, -1.224646799147353454E-16, 0.000000000000000000 ) ) ;
#3835 = ORIENTED_EDGE ( 'NONE', *, *, #10679, .F. ) ;
#3836 = CARTESIAN_POINT ( 'NONE',  ( -0.5525004126151165096, 0.09742072959660473541, 0.1771653543307086520 ) ) ;
#3837 = CIRCLE ( 'NONE', #25481, 0.6299212598425196763 ) ;
#3838 = CARTESIAN_POINT ( 'NONE',  ( -0.02190250779246035590, 0.3346456692913385988, 1.953740157480315043 ) ) ;
#3839 = CARTESIAN_POINT ( 'NONE',  ( 0.1327036767636163017, -0.4954415918535808872, -1.550196850393700920 ) ) ;
#3840 = DIRECTION ( 'NONE',  ( 1.000000000000000000, 0.000000000000000000, 0.000000000000000000 ) ) ;
#3841 = CARTESIAN_POINT ( 'NONE',  ( 0.5476281405333121022, -0.07214854559198019546, 0.9399606299212598381 ) ) ;
#3842 = DIRECTION ( 'NONE',  ( 0.000000000000000000, 0.000000000000000000, 1.000000000000000000 ) ) ;
#3843 = DIRECTION ( 'NONE',  ( 0.000000000000000000, 0.3746092808414298592, 0.9271827687718677824 ) ) ;
#3844 = VERTEX_POINT ( 'NONE', #3328 ) ;
#3845 = CARTESIAN_POINT ( 'NONE',  ( 0.2181214148710974021, 0.2842163005027489864, -3.115157480314961091 ) ) ;
#3846 = VECTOR ( 'NONE', #3403, 39.37007874015748143 ) ;
#3847 = EDGE_CURVE ( 'NONE', #8860, #3368, #16199, .T. ) ;
#3848 = DIRECTION ( 'NONE',  ( 0.000000000000000000, 0.000000000000000000, 1.000000000000000000 ) ) ;
#3849 = CARTESIAN_POINT ( 'NONE',  ( 0.5144751499634915293, 0.1379104267273083551, 1.747047244094488194 ) ) ;
#3850 = EDGE_LOOP ( 'NONE', ( #3032, #12389 ) ) ;
#3851 = AXIS2_PLACEMENT_3D ( 'NONE', #11182, #4553, #19804 ) ;
#3852 = CARTESIAN_POINT ( 'NONE',  ( 0.03349795313024148125, 0.5118110236220473341, -1.550196850393700920 ) ) ;
#3853 = DIRECTION ( 'NONE',  ( -0.1758653632939320421, 0.000000000000000000, 0.9844142288658231932 ) ) ;
#3854 = AXIS2_PLACEMENT_3D ( 'NONE', #1166, #22627, #5968 ) ;
#3855 = CARTESIAN_POINT ( 'NONE',  ( 0.3561571326799479742, 1.175382753584212514, -0.5166459152402519406 ) ) ;
#3856 = CARTESIAN_POINT ( 'NONE',  ( 0.000000000000000000, 0.07874015748662489822, 0.000000000000000000 ) ) ;
#3857 = CARTESIAN_POINT ( 'NONE',  ( -0.2662775206742153955, -0.4613022222208275624, 1.747047244094488194 ) ) ;
#3858 = ORIENTED_EDGE ( 'NONE', *, *, #25706, .T. ) ;
#3859 = CARTESIAN_POINT ( 'NONE',  ( 0.7874015748031496509, -5.862181872598426086E-06, -1.869015748010449007 ) ) ;
#3860 = ORIENTED_EDGE ( 'NONE', *, *, #12938, .F. ) ;
#3861 = EDGE_CURVE ( 'NONE', #26623, #1745, #13934, .T. ) ;
#3862 = CARTESIAN_POINT ( 'NONE',  ( -0.6086690512655491547, -0.5056979702033415069, -0.9923584033843172447 ) ) ;
#3863 = CARTESIAN_POINT ( 'NONE',  ( -0.5819147541874519769, -0.6280848967520352710, -0.9045786101298314286 ) ) ;
#3864 = CARTESIAN_POINT ( 'NONE',  ( 0.000000000000000000, 0.8267716535433071723, 0.02362204724409448786 ) ) ;
#3865 = CARTESIAN_POINT ( 'NONE',  ( 0.07874015748031489015, 0.1968503937007874127, -3.272637795275590733 ) ) ;
#3866 = DIRECTION ( 'NONE',  ( 0.000000000000000000, -1.000000000000000000, 0.000000000000000000 ) ) ;
#3867 = EDGE_CURVE ( 'NONE', #9254, #22901, #4394, .T. ) ;
#3868 = VERTEX_POINT ( 'NONE', #7738 ) ;
#3869 = AXIS2_PLACEMENT_3D ( 'NONE', #13603, #22220, #24208 ) ;
#3870 = DIRECTION ( 'NONE',  ( 0.000000000000000000, 0.000000000000000000, 1.000000000000000000 ) ) ;
#3871 = CARTESIAN_POINT ( 'NONE',  ( -0.1110236220424516002, 0.000000000000000000, 0.6299212598425196763 ) ) ;
#3872 = CARTESIAN_POINT ( 'NONE',  ( -0.4061284506584276199, -0.2351468520616558922, 0.07637795275590551769 ) ) ;
#3873 = B_SPLINE_CURVE_WITH_KNOTS ( 'NONE', 3,
 ( #18048, #11443, #11862, #9045, #26280, #7206, #581, #2806, #15694, #6946, #13699, #20064, #7078, #17659, #24297, #718, #15568, #13418 ),
 .UNSPECIFIED., .F., .F.,
 ( 4, 2, 2, 2, 2, 2, 2, 2, 4 ),
 ( 0.5000000000000000000, 0.5625000000000000000, 0.6250000000000000000, 0.6875000000000000000, 0.7500000000000000000, 0.8125000000000000000, 0.8750000000000000000, 0.9375000000000000000, 1.000000000000000000 ),
 .UNSPECIFIED. ) ;
#3874 = CARTESIAN_POINT ( 'NONE',  ( 0.4669911931914907388, -0.1585706980422228185, -1.569881889763779625 ) ) ;
#3875 = EDGE_CURVE ( 'NONE', #5524, #15921, #14518, .T. ) ;
#3876 = CARTESIAN_POINT ( 'NONE',  ( -0.3929158813954686247, -0.2268989272875759633, -1.934055118110236338 ) ) ;
#3877 = CIRCLE ( 'NONE', #710, 0.4692913385826771866 ) ;
#3878 = CARTESIAN_POINT ( 'NONE',  ( -0.4351030398461734339, 0.1477428134820354677, -1.928289503579158959 ) ) ;
#3879 = EDGE_CURVE ( 'NONE', #13155, #23967, #1753, .T. ) ;
#3880 = AXIS2_PLACEMENT_3D ( 'NONE', #5456, #3307, #11949 ) ;
#3881 = CARTESIAN_POINT ( 'NONE',  ( -0.5072939182192724994, -0.4034160323192637621, -0.1660794105494917405 ) ) ;
#3882 = DIRECTION ( 'NONE',  ( 0.000000000000000000, 0.000000000000000000, -1.000000000000000000 ) ) ;
#3883 = CARTESIAN_POINT ( 'NONE',  ( 0.4612490782035170156, 0.2663596103035609786, 1.747047244094488194 ) ) ;
#3884 = ORIENTED_EDGE ( 'NONE', *, *, #5984, .T. ) ;
#3885 = CARTESIAN_POINT ( 'NONE',  ( 0.3937007874015748254, 0.000000000000000000, -3.036417322828325105 ) ) ;
#3886 = VERTEX_POINT ( 'NONE', #14385 ) ;
#3887 = DIRECTION ( 'NONE',  ( 0.000000000000000000, 0.000000000000000000, 1.000000000000000000 ) ) ;
#3888 = CARTESIAN_POINT ( 'NONE',  ( 0.4121125639456494349, -0.2386018002044008601, 0.2330651857782768399 ) ) ;
#3889 = CARTESIAN_POINT ( 'NONE',  ( 0.4446020952038907681, 5.549066237130534971E-17, -1.934055118110236338 ) ) ;
#3890 = CARTESIAN_POINT ( 'NONE',  ( -0.3074993854542726890, 0.1775730735577450703, 1.953740157480315043 ) ) ;
#3891 = ORIENTED_EDGE ( 'NONE', *, *, #11596, .T. ) ;
#3892 = VERTEX_POINT ( 'NONE', #24953 ) ;
#3893 = CARTESIAN_POINT ( 'NONE',  ( -0.4457380174055288191, -0.4863213126542877962, -0.3953166246891253732 ) ) ;
#3894 = DIRECTION ( 'NONE',  ( 0.000000000000000000, 1.000000000000000000, 0.000000000000000000 ) ) ;
#3895 = AXIS2_PLACEMENT_3D ( 'NONE', #12443, #1151, #14003 ) ;
#3896 = CARTESIAN_POINT ( 'NONE',  ( 0.000000000000000000, 0.5610236220472440971, 0.1771653543307086520 ) ) ;
#3897 = ORIENTED_EDGE ( 'NONE', *, *, #14924, .T. ) ;
#3898 = DIRECTION ( 'NONE',  ( 1.000000000000000000, 0.000000000000000000, 0.000000000000000000 ) ) ;
#3899 = CARTESIAN_POINT ( 'NONE',  ( 0.000000000000000000, 0.07874015748031491790, -1.692913385826771533 ) ) ;
#3900 = ADVANCED_FACE ( 'NONE', ( #22994 ), #20710, .F. ) ;
#3901 = AXIS2_PLACEMENT_3D ( 'NONE', #22366, #2988, #20243 ) ;
#3902 = EDGE_CURVE ( 'NONE', #11779, #25825, #25203, .T. ) ;
#3903 = CARTESIAN_POINT ( 'NONE',  ( -0.2180698645301767380, -0.2842490391651532611, -3.115157480314960647 ) ) ;
#3904 = CARTESIAN_POINT ( 'NONE',  ( -0.5368353335967092077, -0.1442704874421231187, 0.9202755905511812440 ) ) ;
#3905 = CARTESIAN_POINT ( 'NONE',  ( -0.1574803149606299191, 0.000000000000000000, 0.000000000000000000 ) ) ;
#3906 = FACE_OUTER_BOUND ( 'NONE', #14752, .T. ) ;
#3907 = DIRECTION ( 'NONE',  ( 0.000000000000000000, 0.000000000000000000, 1.000000000000000000 ) ) ;
#3908 = CARTESIAN_POINT ( 'NONE',  ( 0.5309636003393858328, 0.6336838567619331730, -0.5358812336713733027 ) ) ;
#3909 = CARTESIAN_POINT ( 'NONE',  ( 0.1520645003680120011, -0.1970746732787106437, -0.4530975572029189435 ) ) ;
#3910 = EDGE_LOOP ( 'NONE', ( #15781, #1259, #839, #24102 ) ) ;
#3911 = AXIS2_PLACEMENT_3D ( 'NONE', #10727, #7915, #27261 ) ;
#3912 = DIRECTION ( 'NONE',  ( 0.000000000000000000, 0.000000000000000000, 1.000000000000000000 ) ) ;
#3913 = EDGE_LOOP ( 'NONE', ( #12682, #15515, #133, #1463 ) ) ;
#3914 = ORIENTED_EDGE ( 'NONE', *, *, #13598, .F. ) ;
#3915 = CIRCLE ( 'NONE', #4809, 0.4055118110236220486 ) ;
#3916 = CARTESIAN_POINT ( 'NONE',  ( 0.000000000000000000, 0.000000000000000000, 0.1992125984251968684 ) ) ;
#3917 = SURFACE_STYLE_FILL_AREA ( #27659 ) ;
#3918 = APPLICATION_PROTOCOL_DEFINITION ( 'draft international standard', 'automotive_design', 1998, #3105 ) ;
#3919 = CARTESIAN_POINT ( 'NONE',  ( -0.2362204724409449064, -1.131889763779527547, 1.386165176200252194E-16 ) ) ;
#3920 = CARTESIAN_POINT ( 'NONE',  ( -0.4069448477556031341, -0.3121994997598085408, 1.747047244094488194 ) ) ;
#3921 = ORIENTED_EDGE ( 'NONE', *, *, #15046, .F. ) ;
#3922 = EDGE_CURVE ( 'NONE', #11887, #24839, #745, .T. ) ;
#3923 = CIRCLE ( 'NONE', #15647, 0.5531496062992126150 ) ;
#3924 = VERTEX_POINT ( 'NONE', #11198 ) ;
#3925 = CARTESIAN_POINT ( 'NONE',  ( -0.2272836761398000505, 0.2962590301041647667, -3.115157480314960647 ) ) ;
#3926 = ORIENTED_EDGE ( 'NONE', *, *, #25191, .F. ) ;
#3927 = DIRECTION ( 'NONE',  ( -1.000000000000000000, 0.000000000000000000, 0.000000000000000000 ) ) ;
#3928 = DIRECTION ( 'NONE',  ( -1.000000000000000000, 0.000000000000000000, 0.000000000000000000 ) ) ;
#3929 = ORIENTED_EDGE ( 'NONE', *, *, #15264, .F. ) ;
#3930 = CARTESIAN_POINT ( 'NONE',  ( 0.4055307389460929279, 4.966319214061935299E-17, -0.1111195235210984261 ) ) ;
#3931 = B_SPLINE_CURVE_WITH_KNOTS ( 'NONE', 3,
 ( #12660, #21291, #1927, #25662, #6316, #21427, #2065, #17591, #11098, #4593, #26207, #641, #24226, #11369, #2872, #19987, #3007, #7004 ),
 .UNSPECIFIED., .F., .F.,
 ( 4, 2, 2, 2, 2, 2, 2, 2, 4 ),
 ( 0.5000000000000000000, 0.5625000000000000000, 0.6250000000000000000, 0.6875000000000000000, 0.7500000000000000000, 0.8125000000000000000, 0.8750000000000001110, 0.9375000000000000000, 1.000000000000000000 ),
 .UNSPECIFIED. ) ;
#3932 = CARTESIAN_POINT ( 'NONE',  ( -0.1677079028045370956, -0.2904160862623674233, 1.973425196850393970 ) ) ;
#3933 = ORIENTED_EDGE ( 'NONE', *, *, #16910, .F. ) ;
#3934 = VERTEX_POINT ( 'NONE', #19157 ) ;
#3935 = CARTESIAN_POINT ( 'NONE',  ( -0.2466292688015410683, 0.4270824798167730529, -1.550196850393700920 ) ) ;
#3936 = DIRECTION ( 'NONE',  ( 0.000000000000000000, -1.000000000000000000, 0.000000000000000000 ) ) ;
#3937 = DIRECTION ( 'NONE',  ( -0.000000000000000000, 1.000000000000000000, -0.000000000000000000 ) ) ;
#3938 = VERTEX_POINT ( 'NONE', #362 ) ;
#3939 = EDGE_LOOP ( 'NONE', ( #8054, #9658 ) ) ;
#3940 = ( BOUNDED_CURVE ( )  B_SPLINE_CURVE ( 2, ( #2272, #21775, #26278 ),
 .UNSPECIFIED., .F., .T. ) 
 B_SPLINE_CURVE_WITH_KNOTS ( ( 3, 3 ),
 ( 0.000000000000000000, 0.1168436138077914160 ),
 .UNSPECIFIED. ) 
 CURVE ( )  GEOMETRIC_REPRESENTATION_ITEM ( )  RATIONAL_B_SPLINE_CURVE ( ( 1.000000000000000000, 1.077350269189623067, 1.077350269189623067 ) ) 
 REPRESENTATION_ITEM ( '' )  ) ;
#3941 = CIRCLE ( 'NONE', #9798, 0.6881889763779527325 ) ;
#3942 = CARTESIAN_POINT ( 'NONE',  ( -0.4783464566929133688, 0.9448818897637796255, -1.639108661417322569E-17 ) ) ;
#3943 = CARTESIAN_POINT ( 'NONE',  ( 0.1431849087165211198, -0.4219262446670075661, -1.934055118110236338 ) ) ;
#3944 = ORIENTED_EDGE ( 'NONE', *, *, #4192, .F. ) ;
#3945 = CARTESIAN_POINT ( 'NONE',  ( 0.4922996667774506840, 0.08741303158498647807, 0.1259302777228524794 ) ) ;
#3946 = ORIENTED_EDGE ( 'NONE', *, *, #16858, .F. ) ;
#3947 = PRODUCT_DEFINITION_SHAPE ( 'NONE', 'NONE',  #16541 ) ;
#3948 = ORIENTED_EDGE ( 'NONE', *, *, #2848, .T. ) ;
#3949 = CARTESIAN_POINT ( 'NONE',  ( 0.1491281042588008532, -0.2312610231601890387, -0.4194211939771484432 ) ) ;
#3950 = DIRECTION ( 'NONE',  ( 1.000000000000000000, 0.000000000000000000, 0.000000000000000000 ) ) ;
#3951 = DIRECTION ( 'NONE',  ( 0.000000000000000000, 0.000000000000000000, 1.000000000000000000 ) ) ;
#3952 = CARTESIAN_POINT ( 'NONE',  ( -0.09842519685039370636, -0.07874015748031495954, -0.04546065111729338803 ) ) ;
#3953 = DIRECTION ( 'NONE',  ( 0.000000000000000000, -1.000000000000000000, 0.000000000000000000 ) ) ;
#3954 = CARTESIAN_POINT ( 'NONE',  ( -0.5585908902305192214, -0.3463899499700468509, 0.1889404979411018481 ) ) ;
#3955 = DIRECTION ( 'NONE',  ( -1.000000000000000000, 0.000000000000000000, 0.000000000000000000 ) ) ;
#3956 = DIRECTION ( 'NONE',  ( 0.000000000000000000, 0.000000000000000000, -1.000000000000000000 ) ) ;
#3957 = ADVANCED_FACE ( 'NONE', ( #26181 ), #21610, .F. ) ;
#3958 = EDGE_CURVE ( 'NONE', #8887, #18279, #12135, .T. ) ;
#3959 = FACE_BOUND ( 'NONE', #21442, .T. ) ;
#3960 = EDGE_LOOP ( 'NONE', ( #697, #25923 ) ) ;
#3961 = ORIENTED_EDGE ( 'NONE', *, *, #5628, .T. ) ;
#3962 = CIRCLE ( 'NONE', #3476, 0.8163976377952752994 ) ;
#3963 = DIRECTION ( 'NONE',  ( -0.000000000000000000, -0.000000000000000000, -1.000000000000000000 ) ) ;
#3964 = EDGE_CURVE ( 'NONE', #19596, #7184, #4695, .T. ) ;
#3965 = CARTESIAN_POINT ( 'NONE',  ( 0.1918813796216842782, -0.5271897577243779276, 0.07676968503937006694 ) ) ;
#3966 = ORIENTED_EDGE ( 'NONE', *, *, #19654, .T. ) ;
#3967 = DIRECTION ( 'NONE',  ( -1.000000000000000000, 0.000000000000000000, 0.000000000000000000 ) ) ;
#3968 = EDGE_CURVE ( 'NONE', #27306, #16609, #24749, .T. ) ;
#3969 = ADVANCED_FACE ( 'NONE', ( #25527 ), #18427, .T. ) ;
#3970 = CARTESIAN_POINT ( 'NONE',  ( -0.2992781133269515892, -0.6197069291944330427, 0.1322834645669291320 ) ) ;
#3971 = CARTESIAN_POINT ( 'NONE',  ( 0.2762247810519147251, 0.4783323773986423166, 0.9202755905511811330 ) ) ;
#3972 = EDGE_LOOP ( 'NONE', ( #24758, #13354 ) ) ;
#3973 = CARTESIAN_POINT ( 'NONE',  ( -0.5905511811023621549, -0.6348133144914153148, 0.8891632684400255782 ) ) ;
#3974 = ORIENTED_EDGE ( 'NONE', *, *, #20018, .T. ) ;
#3975 = CARTESIAN_POINT ( 'NONE',  ( 0.5383630292499967940, 0.4286833100733393742, 0.3401591245381551110 ) ) ;
#3976 = CARTESIAN_POINT ( 'NONE',  ( 0.4563437505065279232, 0.07988585396532887906, 0.2048502514943769115 ) ) ;
#3977 = CARTESIAN_POINT ( 'NONE',  ( -0.4055118110236220486, -0.4724409448818898127, -0.8182917201112815953 ) ) ;
#3978 = CIRCLE ( 'NONE', #19758, 0.6889763779527560139 ) ;
#3979 = DIRECTION ( 'NONE',  ( 0.000000000000000000, 0.000000000000000000, -1.000000000000000000 ) ) ;
#3980 = AXIS2_PLACEMENT_3D ( 'NONE', #17523, #27720, #8365 ) ;
#3981 = ORIENTED_EDGE ( 'NONE', *, *, #2973, .F. ) ;
#3982 = CARTESIAN_POINT ( 'NONE',  ( -0.1189624676717059848, -0.3253923344978159604, 0.1377952755905513249 ) ) ;
#3983 = ORIENTED_EDGE ( 'NONE', *, *, #3922, .T. ) ;
#3984 = CIRCLE ( 'NONE', #14349, 0.1298643763538141760 ) ;
#3985 = B_SPLINE_CURVE_WITH_KNOTS ( 'NONE', 3,
 ( #20427, #7569, #17869, #17996 ),
 .UNSPECIFIED., .F., .F.,
 ( 4, 4 ),
 ( 0.6902184472752670441, 0.6915327610580708217 ),
 .UNSPECIFIED. ) ;
#3986 = CARTESIAN_POINT ( 'NONE',  ( 0.01928643301569668220, -0.07978627494126659669, -0.4680802598521938696 ) ) ;
#3987 = CARTESIAN_POINT ( 'NONE',  ( -0.5417097841048968965, 0.1839420097223028183, 0.9399606299212598381 ) ) ;
#3988 = AXIS2_PLACEMENT_3D ( 'NONE', #5088, #13709, #17926 ) ;
#3989 = CARTESIAN_POINT ( 'NONE',  ( 0.000000000000000000, 0.000000000000000000, -0.2618110236220472231 ) ) ;
#3990 = VERTEX_POINT ( 'NONE', #17820 ) ;
#3991 = CARTESIAN_POINT ( 'NONE',  ( -0.2362017869178774654, 0.2693781226336497969, -3.115157480314962424 ) ) ;
#3992 = ADVANCED_FACE ( 'NONE', ( #13174 ), #8230, .T. ) ;
#3993 = EDGE_CURVE ( 'NONE', #3726, #15200, #17111, .T. ) ;
#3994 = SURFACE_STYLE_USAGE ( .BOTH. , #27444 ) ;
#3995 = EDGE_CURVE ( 'NONE', #26096, #10570, #24430, .T. ) ;
#3996 = AXIS2_PLACEMENT_3D ( 'NONE', #161, #4361, #418 ) ;
#3997 = ORIENTED_EDGE ( 'NONE', *, *, #24206, .F. ) ;
#3998 = CIRCLE ( 'NONE', #21136, 0.2952755905511810774 ) ;
#3999 = CARTESIAN_POINT ( 'NONE',  ( -0.4954415918535620134, 0.1327036767636087800, -1.550196850393700920 ) ) ;
#4000 = CARTESIAN_POINT ( 'NONE',  ( -0.1481194149836671525, -0.5525858403826198195, 0.9399606299212598381 ) ) ;
#4001 = EDGE_CURVE ( 'NONE', #21690, #5829, #13698, .T. ) ;
#4002 = CARTESIAN_POINT ( 'NONE',  ( -0.09842519685039370636, -1.570035826771653483E-17, -0.09092130223458683158 ) ) ;
#4003 = CARTESIAN_POINT ( 'NONE',  ( 0.000000000000000000, 0.000000000000000000, -4.330708661396418080 ) ) ;
#4004 = DIRECTION ( 'NONE',  ( -1.000000000000000000, 0.000000000000000000, 0.000000000000000000 ) ) ;
#4005 = CARTESIAN_POINT ( 'NONE',  ( 0.3122765577851944196, 0.4068916527368734437, -1.550196850393701142 ) ) ;
#4006 = DIRECTION ( 'NONE',  ( 0.000000000000000000, -0.9659258263664933786, -0.2588190448135661570 ) ) ;
#4007 = VERTEX_POINT ( 'NONE', #2805 ) ;
#4008 = ADVANCED_FACE ( 'NONE', ( #11441 ), #20198, .F. ) ;
#4009 = CARTESIAN_POINT ( 'NONE',  ( -0.6050289243185338339, -0.5969388012301621860, -0.9446411342989878834 ) ) ;
#4010 = AXIS2_PLACEMENT_3D ( 'NONE', #17654, #27861, #13413 ) ;
#4011 = VECTOR ( 'NONE', #2594, 39.37007874015748143 ) ;
#4012 = CARTESIAN_POINT ( 'NONE',  ( -0.3661417322834645272, 0.9448818897637796255, -0.1771653543307086520 ) ) ;
#4013 = DIRECTION ( 'NONE',  ( 1.147443000000000016E-15, 1.000000000000000000, -1.224646799147353207E-16 ) ) ;
#4014 = DIRECTION ( 'NONE',  ( 0.000000000000000000, 1.000000000000000000, 0.000000000000000000 ) ) ;
#4015 = ORIENTED_EDGE ( 'NONE', *, *, #12014, .T. ) ;
#4016 = PLANE ( 'NONE',  #10735 ) ;
#4017 = FACE_OUTER_BOUND ( 'NONE', #3179, .T. ) ;
#4018 = UNCERTAINTY_MEASURE_WITH_UNIT (LENGTH_MEASURE( 1.000000000000000082E-05 ), #20102, 'distance_accuracy_value', 'NONE') ;
#4019 = CARTESIAN_POINT ( 'NONE',  ( 0.000000000000000000, 0.000000000000000000, 2.090519358671640647E-11 ) ) ;
#4020 = CARTESIAN_POINT ( 'NONE',  ( -0.3030032861725269200, 0.3454440660767091886, -1.928289503579165620 ) ) ;
#4021 = AXIS2_PLACEMENT_3D ( 'NONE', #24533, #11277, #15663 ) ;
#4022 = CARTESIAN_POINT ( 'NONE',  ( -0.3334645669291338987, 1.286842404713327115, -0.9809137335991812146 ) ) ;
#4023 = AXIS2_PLACEMENT_3D ( 'NONE', #9883, #3089, #20063 ) ;
#4024 = EDGE_CURVE ( 'NONE', #1758, #4513, #4910, .T. ) ;
#4025 = EDGE_LOOP ( 'NONE', ( #15939, #13089, #26409, #6919 ) ) ;
#4026 = CARTESIAN_POINT ( 'NONE',  ( -0.5252801253069795395, -0.3531373716088681003, -0.1448790496363011882 ) ) ;
#4027 = CARTESIAN_POINT ( 'NONE',  ( 0.03008364706454716778, 0.1136516277932334562, 0.1968503937007874127 ) ) ;
#4028 = CARTESIAN_POINT ( 'NONE',  ( -0.03478633594543645985, -0.5314960629921260393, 1.747047244094488194 ) ) ;
#4029 = ADVANCED_FACE ( 'NONE', ( #16112 ), #863, .T. ) ;
#4030 = EDGE_LOOP ( 'NONE', ( #13868, #12961, #18175, #3423 ) ) ;
#4031 = CARTESIAN_POINT ( 'NONE',  ( 0.000000000000000000, 0.000000000000000000, 0.02362204724409448786 ) ) ;
#4032 = EDGE_LOOP ( 'NONE', ( #13615, #17061 ) ) ;
#4033 = ORIENTED_EDGE ( 'NONE', *, *, #2149, .F. ) ;
#4034 = ORIENTED_EDGE ( 'NONE', *, *, #13927, .F. ) ;
#4035 = PLANE ( 'NONE',  #25072 ) ;
#4036 = DIRECTION ( 'NONE',  ( 0.000000000000000000, 0.000000000000000000, 1.000000000000000000 ) ) ;
#4037 = CARTESIAN_POINT ( 'NONE',  ( 0.03937007874015747977, -0.3346456692913385988, 4.098227477461615257E-17 ) ) ;
#4038 = DIRECTION ( 'NONE',  ( 0.000000000000000000, 0.000000000000000000, -1.000000000000000000 ) ) ;
#4039 = AXIS2_PLACEMENT_3D ( 'NONE', #2786, #15416, #312 ) ;
#4040 = CARTESIAN_POINT ( 'NONE',  ( 0.3429980251342366060, 0.09187177619658697114, 1.953740157480315043 ) ) ;
#4041 = CARTESIAN_POINT ( 'NONE',  ( -0.6260402177881045915, -0.06877927659531429816, -0.2391228434390870461 ) ) ;
#4042 = CIRCLE ( 'NONE', #5861, 0.4724409448465559103 ) ;
#4043 = CARTESIAN_POINT ( 'NONE',  ( 0.000000000000000000, 0.000000000000000000, 0.3401574803149606252 ) ) ;
#4044 = CIRCLE ( 'NONE', #17972, 0.3771653543307086909 ) ;
#4045 = VERTEX_POINT ( 'NONE', #18047 ) ;
#4046 = ORIENTED_EDGE ( 'NONE', *, *, #6905, .F. ) ;
#4047 = CARTESIAN_POINT ( 'NONE',  ( 0.000000000000000000, 0.000000000000000000, 0.07637795275590551769 ) ) ;
#4048 = DIRECTION ( 'NONE',  ( 0.000000000000000000, 1.000000000000000000, 0.000000000000000000 ) ) ;
#4049 = EDGE_CURVE ( 'NONE', #26227, #527, #10674, .T. ) ;
#4050 = CARTESIAN_POINT ( 'NONE',  ( 0.3535721684718142188, -0.1200583359873150652, -3.115157480314960647 ) ) ;
#4051 = CARTESIAN_POINT ( 'NONE',  ( -2.185478346456693112E-16, -0.6299212598071869396, 0.000000000000000000 ) ) ;
#4052 = DIRECTION ( 'NONE',  ( 0.000000000000000000, -1.000000000000000000, 0.000000000000000000 ) ) ;
#4053 = CARTESIAN_POINT ( 'NONE',  ( 0.1516263115863346334, 0.2937912646890004087, -0.3972688187320929099 ) ) ;
#4054 = DIRECTION ( 'NONE',  ( -1.000000000000000000, 0.000000000000000000, 0.000000000000000000 ) ) ;
#4055 = FACE_OUTER_BOUND ( 'NONE', #10449, .T. ) ;
#4056 = DIRECTION ( 'NONE',  ( 0.000000000000000000, 1.000000000000000000, 0.000000000000000000 ) ) ;
#4057 = TOROIDAL_SURFACE ( 'NONE', #8129, 0.5610236220472440971, 0.1003937007874015908 ) ;
#4058 = ORIENTED_EDGE ( 'NONE', *, *, #13801, .F. ) ;
#4059 = CARTESIAN_POINT ( 'NONE',  ( 0.2860025288258006282, 0.4954757973262963189, 0.9399606299212598381 ) ) ;
#4060 = ADVANCED_FACE ( 'NONE', ( #1244 ), #7157, .T. ) ;
#4061 = VECTOR ( 'NONE', #262, 39.37007874015748854 ) ;
#4062 = ORIENTED_EDGE ( 'NONE', *, *, #15737, .F. ) ;
#4063 = CARTESIAN_POINT ( 'NONE',  ( -0.4798812372167961526, 0.2895448272006467261, -0.2870126340407198606 ) ) ;
#4064 = ( NAMED_UNIT ( * ) PLANE_ANGLE_UNIT ( ) SI_UNIT ( $, .RADIAN. ) ) ;
#4065 = CARTESIAN_POINT ( 'NONE',  ( -0.5085118447801436625, -0.06699507805368999647, 1.766732283464566899 ) ) ;
#4066 = EDGE_CURVE ( 'NONE', #4877, #4395, #23440, .T. ) ;
#4067 = CARTESIAN_POINT ( 'NONE',  ( -0.2564944395516098874, 0.4441657790107518822, 1.747047244094488194 ) ) ;
#4068 = ORIENTED_EDGE ( 'NONE', *, *, #20406, .T. ) ;
#4069 = EDGE_LOOP ( 'NONE', ( #3739, #21924, #24634, #76, #3096, #7987, #5002 ) ) ;
#4070 = CARTESIAN_POINT ( 'NONE',  ( 0.02339816079119088829, 0.3574975638436101444, -3.115157480314960647 ) ) ;
#4071 = ORIENTED_EDGE ( 'NONE', *, *, #7278, .F. ) ;
#4072 = CARTESIAN_POINT ( 'NONE',  ( -0.4585215200179058037, -0.06002032661671150016, -1.928289503579156516 ) ) ;
#4073 = EDGE_LOOP ( 'NONE', ( #12359, #15976, #13179, #213 ) ) ;
#4074 = CARTESIAN_POINT ( 'NONE',  ( 0.3339160553493882300, 1.066403253539521589, -0.6645352095345236076 ) ) ;
#4075 = CARTESIAN_POINT ( 'NONE',  ( -0.2904160862623674788, 0.1677079028045369846, 1.973425196850393970 ) ) ;
#4076 = ORIENTED_EDGE ( 'NONE', *, *, #6993, .T. ) ;
#4077 = CARTESIAN_POINT ( 'NONE',  ( -0.03220957031754000111, 0.4921259842519685179, -1.550196850393700920 ) ) ;
#4078 = VERTEX_POINT ( 'NONE', #20590 ) ;
#4079 = CARTESIAN_POINT ( 'NONE',  ( 0.000000000000000000, 0.3543307086614172485, 0.000000000000000000 ) ) ;
#4080 = ORIENTED_EDGE ( 'NONE', *, *, #3585, .F. ) ;
#4081 = ORIENTED_EDGE ( 'NONE', *, *, #2043, .T. ) ;
#4082 = CARTESIAN_POINT ( 'NONE',  ( -0.4783464566929133688, -0.4724409448818898127, -0.8182917201112815953 ) ) ;
#4083 = AXIS2_PLACEMENT_3D ( 'NONE', #25482, #23381, #12622 ) ;
#4084 = CIRCLE ( 'NONE', #19402, 0.01377952755905510404 ) ;
#4085 = DIRECTION ( 'NONE',  ( 0.000000000000000000, 0.000000000000000000, -1.000000000000000000 ) ) ;
#4086 = CARTESIAN_POINT ( 'NONE',  ( -0.03190474515785463733, 0.3133989528012832704, -3.641566340106785038 ) ) ;
#4087 = EDGE_LOOP ( 'NONE', ( #18164, #26808, #16298, #25957, #3141, #10241 ) ) ;
#4088 = CARTESIAN_POINT ( 'NONE',  ( -0.05118110236220472370, 0.5570866141732283561, 0.000000000000000000 ) ) ;
#4089 = VERTEX_POINT ( 'NONE', #22707 ) ;
#4090 = TOROIDAL_SURFACE ( 'NONE', #16724, 0.4173228346456693272, 0.02362204724409448786 ) ;
#4091 = CARTESIAN_POINT ( 'NONE',  ( 0.3031496062992122820, 3.784833611538078052E-17, -0.4566929133858267376 ) ) ;
#4092 = DIRECTION ( 'NONE',  ( 0.000000000000000000, 0.000000000000000000, 1.000000000000000000 ) ) ;
#4093 = DIRECTION ( 'NONE',  ( 0.7071067811865480168, -0.7071067811865470176, 0.000000000000000000 ) ) ;
#4094 = CARTESIAN_POINT ( 'NONE',  ( -0.4328487442495566051, -0.8184178445223569964, -0.05697890223968492956 ) ) ;
#4095 = CARTESIAN_POINT ( 'NONE',  ( -0.4585215200179055817, 0.06002032661671174996, -1.928289503579156516 ) ) ;
#4096 = EDGE_CURVE ( 'NONE', #798, #12635, #2896, .T. ) ;
#4097 = CARTESIAN_POINT ( 'NONE',  ( 0.3135473077061334268, 3.969037272548740164E-17, 2.504921259842519898 ) ) ;
#4098 = LINE ( 'NONE', #19058, #17352 ) ;
#4099 = EDGE_CURVE ( 'NONE', #22689, #27836, #10771, .T. ) ;
#4100 = AXIS2_PLACEMENT_3D ( 'NONE', #11265, #13943, #7163 ) ;
#4101 = DIRECTION ( 'NONE',  ( 0.9396926207859082059, -0.3420201433256691015, 0.000000000000000000 ) ) ;
#4102 = CARTESIAN_POINT ( 'NONE',  ( 0.4921259842519685179, 0.000000000000000000, -1.894685039405410665 ) ) ;
#4103 = ORIENTED_EDGE ( 'NONE', *, *, #4417, .F. ) ;
#4104 = ORIENTED_EDGE ( 'NONE', *, *, #24635, .T. ) ;
#4105 = DIRECTION ( 'NONE',  ( 0.000000000000000000, 0.000000000000000000, 1.000000000000000000 ) ) ;
#4106 = DIRECTION ( 'NONE',  ( 0.000000000000000000, -1.000000000000000000, 0.000000000000000000 ) ) ;
#4107 = EDGE_LOOP ( 'NONE', ( #8858, #19737, #10539, #2313 ) ) ;
#4108 = MECHANICAL_DESIGN_GEOMETRIC_PRESENTATION_REPRESENTATION (  '', ( #2724 ), #11773 ) ;
#4109 = CARTESIAN_POINT ( 'NONE',  ( 0.09590060490395689585, -0.1136516277932324709, -0.1968503937007874127 ) ) ;
#4110 = DIRECTION ( 'NONE',  ( -0.9790454724845842893, -0.1018208755700884260, -0.1763589297585410332 ) ) ;
#4111 = DIRECTION ( 'NONE',  ( 0.000000000000000000, 0.000000000000000000, 1.000000000000000000 ) ) ;
#4112 = CARTESIAN_POINT ( 'NONE',  ( 0.5511811023622047445, 0.03607471876262480226, 0.9202755905511811330 ) ) ;
#4113 = ORIENTED_EDGE ( 'NONE', *, *, #7145, .F. ) ;
#4114 = CARTESIAN_POINT ( 'NONE',  ( 0.5322834645669292097, 0.000000000000000000, 0.1322834645669291320 ) ) ;
#4115 = ORIENTED_EDGE ( 'NONE', *, *, #9644, .F. ) ;
#4116 = CARTESIAN_POINT ( 'NONE',  ( 0.2307318466638932919, 0.2741888764671439604, 0.1805249803295128908 ) ) ;
#4117 = DIRECTION ( 'NONE',  ( -0.9790454724845839563, -0.2036417511401769909, 2.493892000000000165E-17 ) ) ;
#4118 = CARTESIAN_POINT ( 'NONE',  ( 0.1279527559055118058, -0.7552056691248124620, -9.248602053916366447E-17 ) ) ;
#4119 = EDGE_CURVE ( 'NONE', #20567, #11128, #8534, .T. ) ;
#4120 = ORIENTED_EDGE ( 'NONE', *, *, #15589, .T. ) ;
#4121 = CARTESIAN_POINT ( 'NONE',  ( -0.1257482708739876276, -0.3439950301903625940, 0.08455817587927060008 ) ) ;
#4122 = CARTESIAN_POINT ( 'NONE',  ( 0.3149606299212598381, 0.000000000000000000, -3.115157480314960647 ) ) ;
#4123 = EDGE_LOOP ( 'NONE', ( #4562, #26365 ) ) ;
#4124 = CARTESIAN_POINT ( 'NONE',  ( 0.2521176338356617697, -0.2211428102655709493, 1.973425196850393970 ) ) ;
#4125 = FACE_OUTER_BOUND ( 'NONE', #4418, .T. ) ;
#4126 = CARTESIAN_POINT ( 'NONE',  ( 0.06200787401574805319, 0.000000000000000000, -4.330708661417323135 ) ) ;
#4127 = DIRECTION ( 'NONE',  ( -1.000000000000000000, 0.000000000000000000, 0.000000000000000000 ) ) ;
#4128 = AXIS2_PLACEMENT_3D ( 'NONE', #9571, #11428, #7062 ) ;
#4129 = CARTESIAN_POINT ( 'NONE',  ( 0.07214854559195596484, 0.5476281405333121022, 0.9399606299212598381 ) ) ;
#4130 = EDGE_CURVE ( 'NONE', #4811, #25542, #26469, .T. ) ;
#4131 = ORIENTED_EDGE ( 'NONE', *, *, #8880, .F. ) ;
#4132 = DIRECTION ( 'NONE',  ( -1.000000000000000000, 0.000000000000000000, 0.000000000000000000 ) ) ;
#4133 = ORIENTED_EDGE ( 'NONE', *, *, #2559, .T. ) ;
#4134 = EDGE_LOOP ( 'NONE', ( #15243, #17542, #1947, #27532 ) ) ;
#4135 = VERTEX_POINT ( 'NONE', #20026 ) ;
#4136 = CARTESIAN_POINT ( 'NONE',  ( 0.4441657790094322711, 0.2564944395535476707, -1.550196850393700920 ) ) ;
#4137 = CARTESIAN_POINT ( 'NONE',  ( 0.2530785775249113079, -0.5130740159361732999, 0.9399606299212600602 ) ) ;
#4138 = DIRECTION ( 'NONE',  ( -1.000000000000000000, -1.224646799147356165E-16, 0.000000000000000000 ) ) ;
#4139 = CARTESIAN_POINT ( 'NONE',  ( 2.664928230027803213, -0.4724409448818898127, -0.9265594366467145848 ) ) ;
#4140 = CARTESIAN_POINT ( 'NONE',  ( -0.0004447986960614348285, 0.5322833254990984031, 0.1322818204150988386 ) ) ;
#4141 = ORIENTED_EDGE ( 'NONE', *, *, #22416, .F. ) ;
#4142 = VERTEX_POINT ( 'NONE', #15662 ) ;
#4143 = COLOUR_RGB ( '', 0.31764706, 0.68627451, 0.89019608) ;
#4144 = CIRCLE ( 'NONE', #3679, 0.06200787401574806013 ) ;
#4145 = CARTESIAN_POINT ( 'NONE',  ( 0.000000000000000000, 0.000000000000000000, 0.1771653543307086520 ) ) ;
#4146 = CARTESIAN_POINT ( 'NONE',  ( -0.5608506285916234901, -0.5625436374635495174, -0.9710811323268585538 ) ) ;
#4147 = DIRECTION ( 'NONE',  ( 0.000000000000000000, 1.000000000000000000, 0.000000000000000000 ) ) ;
#4148 = CARTESIAN_POINT ( 'NONE',  ( 0.4222761783102037536, 0.5043089796494211186, 0.2081850588299743177 ) ) ;
#4149 = DIRECTION ( 'NONE',  ( 1.000000000000000000, 0.000000000000000000, 0.000000000000000000 ) ) ;
#4150 = EDGE_LOOP ( 'NONE', ( #19953, #1191, #3667, #20828, #7453, #14471, #17853, #5870, #22574, #23612, #10773 ) ) ;
#4151 = DIRECTION ( 'NONE',  ( -1.000000000000000000, 0.000000000000000000, 0.000000000000000000 ) ) ;
#4152 = EDGE_CURVE ( 'NONE', #18288, #1952, #14403, .T. ) ;
#4153 = CARTESIAN_POINT ( 'NONE',  ( 0.1491281042588007977, 0.4788599204499175421, 0.009432676026079297657 ) ) ;
#4154 = CARTESIAN_POINT ( 'NONE',  ( -0.2092582568885065775, -0.4359957531186999247, 0.2008762816407658747 ) ) ;
#4155 = EDGE_CURVE ( 'NONE', #11937, #2922, #6286, .T. ) ;
#4156 = CARTESIAN_POINT ( 'NONE',  ( -0.4921259842519685179, -0.03220957031763953954, -1.569881889763779625 ) ) ;
#4157 = EDGE_CURVE ( 'NONE', #15892, #26494, #5820, .T. ) ;
#4158 = CARTESIAN_POINT ( 'NONE',  ( -0.02963280468032113146, 0.4527559054764770385, -1.934055118110236338 ) ) ;
#4159 = EDGE_CURVE ( 'NONE', #12825, #16461, #23873, .T. ) ;
#4160 = CYLINDRICAL_SURFACE ( 'NONE', #18408, 0.3543307086367249448 ) ;
#4161 = CIRCLE ( 'NONE', #7316, 0.3937007874015748254 ) ;
#4162 = B_SPLINE_CURVE_WITH_KNOTS ( 'NONE', 3,
 ( #12876, #14760, #4272, #12465, #14611, #2148, #25743, #23368, #12738, #3991, #27870, #10614, #21646, #10763, #5977, #21366, #6396, #19379, #77, #23214, #8505, #19238, #27732, #3845, #12606, #1868, #10474, #19093, #16989, #14892, #23501, #26414, #2809, #22325 ),
 .UNSPECIFIED., .F., .F.,
 ( 4, 2, 2, 2, 2, 2, 2, 2, 2, 2, 2, 2, 2, 2, 2, 2, 4 ),
 ( 0.000000000000000000, 0.03124999999999996531, 0.06249999999999993061, 0.09374999999999988898, 0.1249999999999998890, 0.1562499999999998612, 0.1874999999999998335, 0.2187499999999998335, 0.2499999999999998335, 0.2812499999999997780, 0.3124999999999997780, 0.3437499999999997224, 0.3749999999999997224, 0.4062499999999997780, 0.4374999999999998335, 0.4687499999999999445, 0.5000000000000000000 ),
 .UNSPECIFIED. ) ;
#4163 = EDGE_LOOP ( 'NONE', ( #9471, #7764, #4924, #22930 ) ) ;
#4164 = ORIENTED_EDGE ( 'NONE', *, *, #25217, .F. ) ;
#4165 = CARTESIAN_POINT ( 'NONE',  ( -0.4881018399981850719, -0.6057852840965571861, 0.08534609957935157531 ) ) ;
#4166 = CARTESIAN_POINT ( 'NONE',  ( 0.000000000000000000, 0.6102362204724409711, 0.2362204724409449064 ) ) ;
#4167 = CARTESIAN_POINT ( 'NONE',  ( 0.4004221243553557907, -0.3512268162760437407, 1.747047244094488194 ) ) ;
#4168 = ORIENTED_EDGE ( 'NONE', *, *, #15874, .T. ) ;
#4169 = CARTESIAN_POINT ( 'NONE',  ( -0.4620608682196346573, 0.08206165078060512208, 0.1992125984251968684 ) ) ;
#4170 = EDGE_LOOP ( 'NONE', ( #7045, #1962, #27253 ) ) ;
#4171 = DIRECTION ( 'NONE',  ( 0.000000000000000000, 0.000000000000000000, 1.000000000000000000 ) ) ;
#4172 = CARTESIAN_POINT ( 'NONE',  ( 0.1110236220424516002, 1.359647233640338808E-17, 0.6299212598425196763 ) ) ;
#4173 = B_SPLINE_SURFACE_WITH_KNOTS ( 'NONE', 2, 3, ( 
 ( #10173, #18791, #27428, #12455, #13285, #11162, #14883, #23715, #5306, #7860, #25215, #20637, #9463, #7499, #5670, #17927, #13710, #878 ),
 ( #18056, #16126, #26999, #20210, #5386, #24866, #3522, #22474, #24722, #12022, #9604, #18209, #26699, #24583, #9318, #14005, #22617, #26846 ),
 ( #15980, #7215, #15833, #3104, #3236, #22332, #20495, #11877, #11736, #9897, #1010, #1153, #27143, #22906, #18354, #16399, #5529, #14151 ) ),
 .UNSPECIFIED., .F., .F., .F.,
 ( 3, 3 ),
 ( 4, 2, 2, 2, 2, 2, 2, 2, 4 ),
 ( 0.000000000000000000, 1.000000000000000000 ),
 ( 4.712388980384689674, 5.105088062083414258, 5.497787143782137953, 5.890486225480861648, 6.283185307179586232, 6.675884388878310816, 7.068583470577034511, 7.461282552275758206, 7.853981633974482790 ),
 .UNSPECIFIED. ) ;
#4174 = DIRECTION ( 'NONE',  ( -1.000000000000000000, 0.000000000000000000, 0.000000000000000000 ) ) ;
#4175 = EDGE_LOOP ( 'NONE', ( #5300, #5732, #25546, #3767, #11176, #16118, #17476, #16891, #14954, #9551, #27254, #17055 ) ) ;
#4176 = VECTOR ( 'NONE', #4885, 39.37007874015748143 ) ;
#4177 = CARTESIAN_POINT ( 'NONE',  ( 0.02319089060378159983, 0.3543307086614173596, 1.953740157480315043 ) ) ;
#4178 = ORIENTED_EDGE ( 'NONE', *, *, #6267, .F. ) ;
#4179 = CONICAL_SURFACE ( 'NONE', #19499, 0.1106489370078740930, 0.08726646250000029414 ) ;
#4180 = CARTESIAN_POINT ( 'NONE',  ( -0.6467180715673140901, -0.02183847761193024803, -0.2362204724409446288 ) ) ;
#4181 = CARTESIAN_POINT ( 'NONE',  ( -0.5724622793728307846, -0.3313001865995510720, 0.1926811207742144816 ) ) ;
#4182 = VERTEX_POINT ( 'NONE', #26651 ) ;
#4183 = CARTESIAN_POINT ( 'NONE',  ( -0.4167985568850881561, 0.07349283109919310664, 0.1377952755905511861 ) ) ;
#4184 = DIRECTION ( 'NONE',  ( 1.000000000000000000, 0.000000000000000000, 0.000000000000000000 ) ) ;
#4185 = EDGE_CURVE ( 'NONE', #24622, #11368, #963, .T. ) ;
#4186 = AXIS2_PLACEMENT_3D ( 'NONE', #19375, #25313, #16985 ) ;
#4187 = CARTESIAN_POINT ( 'NONE',  ( 0.1867299569291683836, 0.3233561589689052940, -3.115157480314960647 ) ) ;
#4188 = CARTESIAN_POINT ( 'NONE',  ( -0.09586345242798399724, 0.2165354330708661734, -3.573990933499928691 ) ) ;
#4189 = FACE_OUTER_BOUND ( 'NONE', #17127, .T. ) ;
#4190 = FACE_OUTER_BOUND ( 'NONE', #26019, .T. ) ;
#4191 = DIRECTION ( 'NONE',  ( -7.017815000000000124E-18, 1.000000000000000000, -1.224646799147353207E-16 ) ) ;
#4192 = EDGE_CURVE ( 'NONE', #7888, #3247, #4462, .T. ) ;
#4193 = CARTESIAN_POINT ( 'NONE',  ( 0.0005963271530354272241, 0.4972008316437019904, 0.1140743250946049531 ) ) ;
#4194 = CARTESIAN_POINT ( 'NONE',  ( -0.6867658503640922119, -0.1559616964386716931, 0.3281099440157777547 ) ) ;
#4195 = AXIS2_PLACEMENT_3D ( 'NONE', #18710, #5744, #7565 ) ;
#4196 = ORIENTED_EDGE ( 'NONE', *, *, #17233, .F. ) ;
#4197 = CARTESIAN_POINT ( 'NONE',  ( 0.5382052855068000241, 0.4288813374988101890, 0.1322810039474933141 ) ) ;
#4198 = DIRECTION ( 'NONE',  ( 1.000000000000000000, 0.000000000000000000, 0.000000000000000000 ) ) ;
#4199 = CARTESIAN_POINT ( 'NONE',  ( 0.03532354024591839031, -0.6299212598425196763, 0.000000000000000000 ) ) ;
#4200 = APPLICATION_PROTOCOL_DEFINITION ( 'draft international standard', 'automotive_design', 1998, #12864 ) ;
#4201 = VECTOR ( 'NONE', #6751, 39.37007874015748143 ) ;
#4202 = CARTESIAN_POINT ( 'NONE',  ( -0.4441657790107744752, -0.2564944395515745823, 1.766732283464566899 ) ) ;
#4203 = CARTESIAN_POINT ( 'NONE',  ( -0.5118110236220472231, 0.03349795313264340019, 1.747047244094488194 ) ) ;
#4204 = EDGE_CURVE ( 'NONE', #23387, #7189, #11665, .T. ) ;
#4205 = VERTEX_POINT ( 'NONE', #11407 ) ;
#4206 = AXIS2_PLACEMENT_3D ( 'NONE', #577, #9172, #11438 ) ;
#4207 = EDGE_LOOP ( 'NONE', ( #15106, #13124 ) ) ;
#4209 = CARTESIAN_POINT ( 'NONE',  ( 0.3102476824511484210, 0.1791601451668926315, -3.115157480314960647 ) ) ;
#4208 = CARTESIAN_POINT ( 'NONE',  ( -0.6239291699148459269, 0.1106940470466721976, 0.1061598535656959191 ) ) ;
#4210 = ORIENTED_EDGE ( 'NONE', *, *, #19484, .T. ) ;
#4211 = ORIENTED_EDGE ( 'NONE', *, *, #14748, .T. ) ;
#4212 = CARTESIAN_POINT ( 'NONE',  ( -0.1704479274145711543, -0.4700505334971128990, 0.1259302777278768770 ) ) ;
#4213 = FACE_OUTER_BOUND ( 'NONE', #20605, .T. ) ;
#4214 = CARTESIAN_POINT ( 'NONE',  ( 0.1482986320106399469, 0.3007905576423889893, 1.973425196850393970 ) ) ;
#4215 = EDGE_LOOP ( 'NONE', ( #10322, #12442 ) ) ;
#4216 = EDGE_LOOP ( 'NONE', ( #13398, #18115 ) ) ;
#4217 = CARTESIAN_POINT ( 'NONE',  ( -0.1585706980422388890, 0.4669911931914605963, -1.550196850393700920 ) ) ;
#4218 = DIRECTION ( 'NONE',  ( 0.000000000000000000, 0.000000000000000000, 1.000000000000000000 ) ) ;
#4219 = VERTEX_POINT ( 'NONE', #7445 ) ;
#4220 = ORIENTED_EDGE ( 'NONE', *, *, #19484, .F. ) ;
#4221 = EDGE_LOOP ( 'NONE', ( #24244, #2218, #3066 ) ) ;
#4222 = CARTESIAN_POINT ( 'NONE',  ( -0.4307823082429378392, 0.000000000000000000, -0.1559029880880275776 ) ) ;
#4223 = ADVANCED_FACE ( 'NONE', ( #5906, #1654 ), #16631, .T. ) ;
#4224 = AXIS2_PLACEMENT_3D ( 'NONE', #21526, #25764, #6415 ) ;
#4225 = CONTEXT_DEPENDENT_SHAPE_REPRESENTATION ( #13226, #5325 ) ;
#4226 = LINE ( 'NONE', #26104, #11288 ) ;
#4227 = DIRECTION ( 'NONE',  ( 1.000000000000000000, 0.000000000000000000, 0.000000000000000000 ) ) ;
#4228 = FACE_OUTER_BOUND ( 'NONE', #1938, .T. ) ;
#4229 = ORIENTED_EDGE ( 'NONE', *, *, #19009, .F. ) ;
#4230 = ADVANCED_FACE ( 'NONE', ( #1793 ), #22983, .T. ) ;
#4231 = AXIS2_PLACEMENT_3D ( 'NONE', #5476, #27092, #20158 ) ;
#4232 = DIRECTION ( 'NONE',  ( 0.000000000000000000, 0.000000000000000000, 1.000000000000000000 ) ) ;
#4233 = AXIS2_PLACEMENT_3D ( 'NONE', #6903, #18150, #22011 ) ;
#4234 = CARTESIAN_POINT ( 'NONE',  ( 0.000000000000000000, 0.000000000000000000, -0.04133858267716535029 ) ) ;
#4235 = DIRECTION ( 'NONE',  ( 0.000000000000000000, 0.000000000000000000, 1.000000000000000000 ) ) ;
#4236 = CARTESIAN_POINT ( 'NONE',  ( -0.3854046260861516138, -1.009161588507168972, -0.2500462002441404263 ) ) ;
#4237 = EDGE_CURVE ( 'NONE', #15069, #804, #19759, .T. ) ;
#4238 = DIRECTION ( 'NONE',  ( -1.000000000000000000, 0.000000000000000000, 0.000000000000000000 ) ) ;
#4239 = CARTESIAN_POINT ( 'NONE',  ( 0.000000000000000000, 0.000000000000000000, -0.4724409448818898127 ) ) ;
#4240 = CLOSED_SHELL ( 'NONE', ( #1830, #13050, #19431, #11481, #22826, #19397, #5725, #6414, #10444, #23680, #12611, #27305, #13808, #2258, #26833, #26614, #7641, #9887, #2109, #11451, #4519, #4609, #3296, #5606, #6419, #15626, #14039, #21511, #9703, #11107, #20369, #24480 ) ) ;
#4241 = EDGE_CURVE ( 'NONE', #15651, #15443, #1710, .T. ) ;
#4242 = CARTESIAN_POINT ( 'NONE',  ( 0.06880207798751564185, 0.1968503937007873850, -3.232982757847921995 ) ) ;
#4243 = ORIENTED_EDGE ( 'NONE', *, *, #3500, .T. ) ;
#4244 = CARTESIAN_POINT ( 'NONE',  ( -0.7874015748031496509, 0.3058301319751310920, -0.2956682880063846164 ) ) ;
#4245 = CARTESIAN_POINT ( 'NONE',  ( 0.000000000000000000, 0.000000000000000000, 0.3425196850393700809 ) ) ;
#4246 = ORIENTED_EDGE ( 'NONE', *, *, #21408, .F. ) ;
#4247 = DIRECTION ( 'NONE',  ( -0.000000000000000000, -0.000000000000000000, -1.000000000000000000 ) ) ;
#4248 = DIRECTION ( 'NONE',  ( 1.000000000000000000, 0.000000000000000000, 0.000000000000000000 ) ) ;
#4249 = CIRCLE ( 'NONE', #25904, 0.05216535433070866590 ) ;
#4250 = CARTESIAN_POINT ( 'NONE',  ( -0.3362148458988422073, 0.4382482975805319092, 0.9202755905511811330 ) ) ;
#4251 = CARTESIAN_POINT ( 'NONE',  ( -0.6562077975700374433, -2.731848031496062854E-17, -0.1574803149606299191 ) ) ;
#4252 = ORIENTED_EDGE ( 'NONE', *, *, #14545, .F. ) ;
#4253 = CARTESIAN_POINT ( 'NONE',  ( -0.4333973147258542991, -0.2509079296564011852, 0.09685039370078740717 ) ) ;
#4254 = DIRECTION ( 'NONE',  ( 0.000000000000000000, 0.000000000000000000, -1.000000000000000000 ) ) ;
#4255 = CARTESIAN_POINT ( 'NONE',  ( 0.6102362204724409711, 0.000000000000000000, 0.2362204724409449064 ) ) ;
#4256 = DIRECTION ( 'NONE',  ( 0.000000000000000000, 0.000000000000000000, -1.000000000000000000 ) ) ;
#4257 = DIRECTION ( 'NONE',  ( 0.000000000000000000, 0.000000000000000000, 1.000000000000000000 ) ) ;
#4258 = EDGE_CURVE ( 'NONE', #24011, #9956, #2670, .T. ) ;
#4259 = CONICAL_SURFACE ( 'NONE', #7865, 0.2938622683360631593, 0.2617993874999998138 ) ;
#4260 = ADVANCED_FACE ( 'NONE', ( #18874 ), #10125, .T. ) ;
#4261 = ORIENTED_EDGE ( 'NONE', *, *, #18963, .F. ) ;
#4262 = CARTESIAN_POINT ( 'NONE',  ( 0.6710470464557933834, -0.1526433524318244195, 0.1322818203437344520 ) ) ;
#4263 = CARTESIAN_POINT ( 'NONE',  ( -0.1230388948646404523, -0.3365682031886393366, 0.09506557084333611130 ) ) ;
#4264 = DIRECTION ( 'NONE',  ( 0.000000000000000000, -1.000000000000000000, 0.000000000000000000 ) ) ;
#4265 = CARTESIAN_POINT ( 'NONE',  ( 0.6478824768876890738, 0.1135474080048673312, 0.2081850588311874306 ) ) ;
#4266 = CARTESIAN_POINT ( 'NONE',  ( 0.4167985568850881561, 0.07349283109919291235, 0.1377952755905511861 ) ) ;
#4267 = DIRECTION ( 'NONE',  ( 0.000000000000000000, 0.000000000000000000, 1.000000000000000000 ) ) ;
#4268 = CIRCLE ( 'NONE', #6503, 0.3346456692913385988 ) ;
#4269 = AXIS2_PLACEMENT_3D ( 'NONE', #3856, #1323, #16998 ) ;
#4270 = DIRECTION ( 'NONE',  ( -0.000000000000000000, -0.000000000000000000, -1.000000000000000000 ) ) ;
#4271 = ORIENTED_EDGE ( 'NONE', *, *, #15237, .T. ) ;
#4272 = CARTESIAN_POINT ( 'NONE',  ( -0.3552036222399427290, 0.04673558830906447692, -3.115157480314960647 ) ) ;
#4273 = ORIENTED_EDGE ( 'NONE', *, *, #1693, .F. ) ;
#4274 = CIRCLE ( 'NONE', #6533, 0.4803149606299212393 ) ;
#4275 = ORIENTED_EDGE ( 'NONE', *, *, #25762, .T. ) ;
#4276 = ADVANCED_FACE ( 'NONE', ( #18446 ), #20262, .F. ) ;
#4277 = CARTESIAN_POINT ( 'NONE',  ( -0.4763861460130774939, -0.1275996891957774104, -1.550196850393700920 ) ) ;
#4278 = CARTESIAN_POINT ( 'NONE',  ( 0.5672083774005964862, -0.07462150385395434349, 0.9399606299212600602 ) ) ;
#4279 = CARTESIAN_POINT ( 'NONE',  ( 0.4620608682196457040, 0.08206165078054626638, 0.07637795275590551769 ) ) ;
#4280 = CARTESIAN_POINT ( 'NONE',  ( 0.5096726623840774906, -0.1170085733297229341, 0.1392975274247515161 ) ) ;
#4281 = CARTESIAN_POINT ( 'NONE',  ( -0.5314960629921260393, 6.402768735150616610E-17, 1.747047244094488194 ) ) ;
#4282 = ORIENTED_EDGE ( 'NONE', *, *, #26906, .F. ) ;
#4283 = LINE ( 'NONE', #9058, #23272 ) ;
#4284 = ORIENTED_EDGE ( 'NONE', *, *, #8725, .T. ) ;
#4285 = AXIS2_PLACEMENT_3D ( 'NONE', #25571, #8469, #12703 ) ;
#4286 = CARTESIAN_POINT ( 'NONE',  ( 0.05001895696127157259, -0.4012255422357954848, -0.3367473437330908426 ) ) ;
#4287 = TOROIDAL_SURFACE ( 'NONE', #7899, 0.6751968503937006982, 0.01377952755905511792 ) ;
#4288 = CARTESIAN_POINT ( 'NONE',  ( -0.4563437504957677526, 0.07988585396341746359, 0.1494804572056230296 ) ) ;
#4289 = CARTESIAN_POINT ( 'NONE',  ( -0.3991696156513685478, 0.4760540497243803681, 0.2574827755769819038 ) ) ;
#4290 = EDGE_LOOP ( 'NONE', ( #7597, #11737 ) ) ;
#4291 = CARTESIAN_POINT ( 'NONE',  ( 0.5007874015748030594, 0.000000000000000000, 0.09685039370078740717 ) ) ;
#4292 = FACE_OUTER_BOUND ( 'NONE', #11102, .T. ) ;
#4293 = LINE ( 'NONE', #11400, #12043 ) ;
#4294 = LINE ( 'NONE', #26176, #14378 ) ;
#4295 = CARTESIAN_POINT ( 'NONE',  ( 0.3252100150720097504, 0.3707612262533033776, -1.550196850393700920 ) ) ;
#4296 = AXIS2_PLACEMENT_3D ( 'NONE', #19164, #16774, #14955 ) ;
#4297 = PRODUCT_DEFINITION_CONTEXT ( 'detailed design', #1154, 'design' ) ;
#4298 = VERTEX_POINT ( 'NONE', #7880 ) ;
#4299 = CARTESIAN_POINT ( 'NONE',  ( 0.2006393256663695779, -0.4069519308876702324, -1.934055118110236338 ) ) ;
#4300 = AXIS2_PLACEMENT_3D ( 'NONE', #16529, #3375, #25007 ) ;
#4301 = DIRECTION ( 'NONE',  ( 0.000000000000000000, 1.000000000000000000, 0.000000000000000000 ) ) ;
#4302 = AXIS2_PLACEMENT_3D ( 'NONE', #2673, #849, #2941 ) ;
#4303 = CARTESIAN_POINT ( 'NONE',  ( -0.4995226175161708859, -0.4941169763608158072, -0.03469573555946992016 ) ) ;
#4304 = DIRECTION ( 'NONE',  ( -1.000000000000000000, 0.000000000000000000, 0.000000000000000000 ) ) ;
#4305 = ADVANCED_FACE ( 'NONE', ( #3771 ), #9411, .F. ) ;
#4306 = LENGTH_MEASURE_WITH_UNIT ( LENGTH_MEASURE( 0.02539999999999999897 ), #16546 ) ;
#4307 = EDGE_CURVE ( 'NONE', #15542, #3371, #12553, .T. ) ;
#4308 = CARTESIAN_POINT ( 'NONE',  ( 0.1520645003680120011, -0.2938566582910456804, 0.3972204521033409486 ) ) ;
#4309 = DIRECTION ( 'NONE',  ( 0.000000000000000000, -1.000000000000000000, 0.000000000000000000 ) ) ;
#4310 = CARTESIAN_POINT ( 'NONE',  ( -0.4446020952038907126, 0.02918571160814592211, -1.934055118110236560 ) ) ;
#4311 = EDGE_CURVE ( 'NONE', #19874, #10834, #13049, .T. ) ;
#4312 = AXIS2_PLACEMENT_3D ( 'NONE', #13964, #10269, #16225 ) ;
#4313 = CARTESIAN_POINT ( 'NONE',  ( -0.7246715730664488042, 0.2518900982766236196, 0.2118286996268641809 ) ) ;
#4314 = ORIENTED_EDGE ( 'NONE', *, *, #22479, .F. ) ;
#4315 = B_SPLINE_CURVE_WITH_KNOTS ( 'NONE', 3,
 ( #7359, #26556, #15979, #24582, #5955, #7645, #3822, #20917, #1844, #3970 ),
 .UNSPECIFIED., .F., .F.,
 ( 4, 2, 2, 2, 4 ),
 ( 0.000000000000000000, 0.2500000000000002776, 0.5000000000000001110, 0.7500000000000000000, 1.000000000000000000 ),
 .UNSPECIFIED. ) ;
#4316 = DIRECTION ( 'NONE',  ( 0.000000000000000000, 0.000000000000000000, -1.000000000000000000 ) ) ;
#4317 = CARTESIAN_POINT ( 'NONE',  ( 0.03736310157557471562, -0.5708661417322835607, 0.9399606299212598381 ) ) ;
#4318 = EDGE_CURVE ( 'NONE', #26847, #26227, #22855, .T. ) ;
#4319 = CARTESIAN_POINT ( 'NONE',  ( -0.3665264996331779601, -0.2116141732283464416, 0.1377952755905511861 ) ) ;
#4320 = EDGE_LOOP ( 'NONE', ( #554, #5455, #23514, #17998, #19948 ) ) ;
#4321 = CARTESIAN_POINT ( 'NONE',  ( -0.6869867706933208140, 0.5354097223591692822, -0.4217158658263621684 ) ) ;
#4322 = CARTESIAN_POINT ( 'NONE',  ( 0.2962590301041581609, -0.2272836761397895311, -3.115157480314960647 ) ) ;
#4323 = AXIS2_PLACEMENT_3D ( 'NONE', #11732, #15831, #24581 ) ;
#4324 = DIRECTION ( 'NONE',  ( 1.000000000000000000, 0.000000000000000000, 0.000000000000000000 ) ) ;
#4325 = FILL_AREA_STYLE ('',( #23421 ) ) ;
#4326 = CARTESIAN_POINT ( 'NONE',  ( -0.2307318466648207722, 0.2741888764682436364, 0.09506557084940545077 ) ) ;
#4327 = FACE_OUTER_BOUND ( 'NONE', #24593, .T. ) ;
#4328 = CARTESIAN_POINT ( 'NONE',  ( 0.000000000000000000, 0.000000000000000000, -3.278217716535432842E-17 ) ) ;
#4329 = AXIS2_PLACEMENT_3D ( 'NONE', #23258, #12223, #12644 ) ;
#4330 = DIMENSIONAL_EXPONENTS ( 1.000000000000000000, 0.000000000000000000, 0.000000000000000000, 0.000000000000000000, 0.000000000000000000, 0.000000000000000000, 0.000000000000000000 ) ;
#4331 = TOROIDAL_SURFACE ( 'NONE', #20105, 0.6102362204724409711, 0.1299212598425196763 ) ;
#4332 = EDGE_LOOP ( 'NONE', ( #27446, #6202 ) ) ;
#4333 = EDGE_CURVE ( 'NONE', #27329, #8591, #12247, .T. ) ;
#4334 = EDGE_LOOP ( 'NONE', ( #26514, #26729, #27046, #19687 ) ) ;
#4335 = DIRECTION ( 'NONE',  ( 0.000000000000000000, 0.000000000000000000, 1.000000000000000000 ) ) ;
#4336 = CARTESIAN_POINT ( 'NONE',  ( 0.2019525613798653640, 0.7328932975451569742, 1.590379927979397374E-17 ) ) ;
#4337 = B_SPLINE_CURVE_WITH_KNOTS ( 'NONE', 3,
 ( #25030, #27296, #25315, #3541, #12170, #20655 ),
 .UNSPECIFIED., .F., .F.,
 ( 4, 2, 4 ),
 ( 0.5000000000000000000, 0.7500000000000000000, 1.000000000000000000 ),
 .UNSPECIFIED. ) ;
#4338 = APPLICATION_PROTOCOL_DEFINITION ( 'draft international standard', 'automotive_design', 1998, #19006 ) ;
#4339 = CARTESIAN_POINT ( 'NONE',  ( -0.03349795313264251895, -0.5118110236220473341, 1.766732283464566899 ) ) ;
#4340 = DIRECTION ( 'NONE',  ( -0.1034422368825631960, 0.9946354626840587798, 0.000000000000000000 ) ) ;
#4341 = ORIENTED_EDGE ( 'NONE', *, *, #14178, .F. ) ;
#4342 = ADVANCED_FACE ( 'NONE', ( #14249, #25104 ), #13866, .T. ) ;
#4343 = ORIENTED_EDGE ( 'NONE', *, *, #15925, .T. ) ;
#4344 = CARTESIAN_POINT ( 'NONE',  ( -0.3551931031211721379, -0.04679574315772278004, -3.115157480314960647 ) ) ;
#4345 = ORIENTED_EDGE ( 'NONE', *, *, #19521, .T. ) ;
#4346 = ORIENTED_EDGE ( 'NONE', *, *, #2909, .T. ) ;
#4347 = CARTESIAN_POINT ( 'NONE',  ( -0.06200787401574805319, 7.593774443531818500E-18, -4.330708661417323135 ) ) ;
#4348 = CARTESIAN_POINT ( 'NONE',  ( -0.2965233727166468602, 0.3524965443697189449, 0.1903859677771958248 ) ) ;
#4349 = EDGE_CURVE ( 'NONE', #7482, #3868, #8097, .T. ) ;
#4350 = CARTESIAN_POINT ( 'NONE',  ( -0.3324885138898245329, -0.04380447413658584976, 1.973425196850393970 ) ) ;
#4351 = VERTEX_POINT ( 'NONE', #6518 ) ;
#4352 = ORIENTED_EDGE ( 'NONE', *, *, #4155, .F. ) ;
#4353 = TOROIDAL_SURFACE ( 'NONE', #21954, 0.3031496062992122820, 0.01181102362204755792 ) ;
#4354 = CARTESIAN_POINT ( 'NONE',  ( 0.6117062799105453808, 0.1085321106658576895, 0.09685039370078740717 ) ) ;
#4355 = ORIENTED_EDGE ( 'NONE', *, *, #1228, .T. ) ;
#4356 = VERTEX_POINT ( 'NONE', #16980 ) ;
#4357 = EDGE_LOOP ( 'NONE', ( #10983, #4487, #18521, #23672 ) ) ;
#4358 = CARTESIAN_POINT ( 'NONE',  ( -0.1715719712210964643, -0.4696414150085483352, 0.1259302777219306335 ) ) ;
#4359 = B_SPLINE_CURVE_WITH_KNOTS ( 'NONE', 3,
 ( #24110, #8853, #15642, #7020, #26355, #2751, #19735, #20282 ),
 .UNSPECIFIED., .F., .F.,
 ( 4, 2, 2, 4 ),
 ( 0.5000000000000000000, 0.7500000000000002220, 0.8750000000000000000, 1.000000000000000000 ),
 .UNSPECIFIED. ) ;
#4360 = PLANE ( 'NONE',  #20753 ) ;
#4361 = DIRECTION ( 'NONE',  ( 0.000000000000000000, 0.000000000000000000, -1.000000000000000000 ) ) ;
#4362 = FACE_BOUND ( 'NONE', #16942, .T. ) ;
#4363 = ORIENTED_EDGE ( 'NONE', *, *, #16536, .F. ) ;
#4364 = EDGE_CURVE ( 'NONE', #18101, #724, #17498, .T. ) ;
#4365 = AXIS2_PLACEMENT_3D ( 'NONE', #16950, #20904, #3953 ) ;
#4366 = CIRCLE ( 'NONE', #14290, 0.3937007874015748254 ) ;
#4367 = CARTESIAN_POINT ( 'NONE',  ( -0.5810616737516007824, 1.098416878720776424, 0.09031125883555725375 ) ) ;
#4368 = AXIS2_PLACEMENT_3D ( 'NONE', #9283, #2386, #11147 ) ;
#4369 = DIRECTION ( 'NONE',  ( 0.000000000000000000, 0.000000000000000000, -1.000000000000000000 ) ) ;
#4370 = LINE ( 'NONE', #13117, #25467 ) ;
#4371 = CYLINDRICAL_SURFACE ( 'NONE', #7410, 0.2952755905511810774 ) ;
#4372 = EDGE_CURVE ( 'NONE', #7546, #21258, #22778, .T. ) ;
#4373 = CARTESIAN_POINT ( 'NONE',  ( 0.01288382760289561411, 0.1968503937007873850, -3.174212598425197207 ) ) ;
#4375 = EDGE_CURVE ( 'NONE', #13737, #23196, #11246, .T. ) ;
#4374 = ORIENTED_EDGE ( 'NONE', *, *, #5024, .T. ) ;
#4376 = CARTESIAN_POINT ( 'NONE',  ( 0.3265485372158890010, -0.1887320510662011952, 0.07637549214372835182 ) ) ;
#4377 = EDGE_CURVE ( 'NONE', #10201, #16332, #26831, .T. ) ;
#4378 = ORIENTED_EDGE ( 'NONE', *, *, #7794, .F. ) ;
#4379 = CIRCLE ( 'NONE', #4458, 0.7500000000000001110 ) ;
#4380 = FACE_BOUND ( 'NONE', #20747, .T. ) ;
#4381 = DIRECTION ( 'NONE',  ( 0.000000000000000000, -1.000000000000000000, 0.000000000000000000 ) ) ;
#4382 = AXIS2_PLACEMENT_3D ( 'NONE', #11586, #24576, #3092 ) ;
#4383 = DIRECTION ( 'NONE',  ( -1.000000000000000000, 0.000000000000000000, 0.000000000000000000 ) ) ;
#4384 = ORIENTED_EDGE ( 'NONE', *, *, #25655, .T. ) ;
#4385 = CARTESIAN_POINT ( 'NONE',  ( -0.5335524835332334792, -0.1429116519061227608, 0.9202755905511811330 ) ) ;
#4386 = EDGE_CURVE ( 'NONE', #2394, #3462, #4044, .T. ) ;
#4387 = CARTESIAN_POINT ( 'NONE',  ( 0.3430989538744064205, 0.06100393589346814194, 0.1589462317967534899 ) ) ;
#4388 = ORIENTED_EDGE ( 'NONE', *, *, #4417, .T. ) ;
#4389 = CARTESIAN_POINT ( 'NONE',  ( -0.4334967711386992772, -0.2507361369899905879, 0.09684874903502814492 ) ) ;
#4390 = CARTESIAN_POINT ( 'NONE',  ( 0.6299212598425196763, 7.714310545810098438E-17, -0.01377952755905511792 ) ) ;
#4391 = TOROIDAL_SURFACE ( 'NONE', #13855, 0.4980314960629921295, 0.01377952755905511792 ) ;
#4392 = DIRECTION ( 'NONE',  ( 0.000000000000000000, 1.000000000000000000, 0.000000000000000000 ) ) ;
#4393 = CARTESIAN_POINT ( 'NONE',  ( 0.1610509776512037416, -0.4407912692718771175, 0.07637795275590551769 ) ) ;
#4394 = B_SPLINE_CURVE_WITH_KNOTS ( 'NONE', 3,
 ( #9844, #23133, #3475, #27514, #14677, #18870, #6045, #14244, #27652, #12104 ),
 .UNSPECIFIED., .F., .F.,
 ( 4, 2, 2, 2, 4 ),
 ( 0.000000000000000000, 0.2500000000000000000, 0.5000000000000000000, 0.7500000000000000000, 1.000000000000000000 ),
 .UNSPECIFIED. ) ;
#4395 = VERTEX_POINT ( 'NONE', #2265 ) ;
#4396 = CARTESIAN_POINT ( 'NONE',  ( -0.0002525749203917322682, 0.6881889763779527325, 0.1322810039474933141 ) ) ;
#4397 = ADVANCED_FACE ( 'NONE', ( #21355 ), #1992, .F. ) ;
#4398 = CARTESIAN_POINT ( 'NONE',  ( 0.1570092758121685861, -0.4330450457732857306, 0.1639447408159873665 ) ) ;
#4399 = FACE_OUTER_BOUND ( 'NONE', #7120, .T. ) ;
#4400 = CARTESIAN_POINT ( 'NONE',  ( -0.07874015748031495954, 0.1968503937007873850, -3.364501312335955063 ) ) ;
#4401 = DIRECTION ( 'NONE',  ( -1.000000000000000000, 0.000000000000000000, 0.000000000000000000 ) ) ;
#4402 = DIRECTION ( 'NONE',  ( 0.000000000000000000, 0.000000000000000000, 1.000000000000000000 ) ) ;
#4403 = DIRECTION ( 'NONE',  ( -0.9790454724845842893, -0.1018208755700880375, -0.1763589297585410332 ) ) ;
#4404 = CARTESIAN_POINT ( 'NONE',  ( -0.0003854097504293205949, 0.4692912202195575477, 0.1992142434433716580 ) ) ;
#4405 = CARTESIAN_POINT ( 'NONE',  ( 0.000000000000000000, 0.4724409448818898127, -1.692913385826771533 ) ) ;
#4406 = CARTESIAN_POINT ( 'NONE',  ( -0.03736310157557561074, 0.5708661417322835607, 0.9399606299212598381 ) ) ;
#4407 = CARTESIAN_POINT ( 'NONE',  ( 0.03359157810863758198, -0.5118124425184569226, -1.550196850393701142 ) ) ;
#4408 = CARTESIAN_POINT ( 'NONE',  ( -0.3338887748335570560, -1.269220122646561588, -0.8285976369166339062 ) ) ;
#4409 = ORIENTED_EDGE ( 'NONE', *, *, #1431, .F. ) ;
#4410 = B_SPLINE_SURFACE_WITH_KNOTS ( 'NONE', 2, 3, ( 
 ( #16141, #18225, #27158, #16277, #26568, #741, #7660, #9329, #24737, #26861, #22490, #15847, #15994, #7227, #5398, #13583, #18508, #13724, #14017, #22629, #24321, #9767, #22345, #11891, #4970, #2971, #18363, #11606, #1169, #20227, #886, #24880, #27014, #9473, #5539, #26712, #14163, #22764, #3391, #22204, #2832, #7372, #24594, #5248, #13870, #3118, #20366, #1024, #1433, #5830, #27582, #23204, #10327, #1860, #18945, #1578, #10045, #4124, #8224, #7942, #23358, #18651, #21218, #16843, #19229, #1996 ),
 ( #6250, #14753, #27432, #27292, #14454, #23065, #3683, #12308, #20933, #10178, #18796, #25451, #25311, #10467, #8087, #16699, #5970, #3838, #12458, #12598, #27724, #21066, #1715, #12004, #5367, #24850, #18042, #574, #11856, #13693, #26538, #22457, #15687, #13990, #22314, #2801, #9170, #11435, #13557, #7481, #11577, #20477, #26978, #1136, #9738, #20193, #14127, #856, #9442, #20058, #7630, #11716, #7343, #22734, #17789, #26408, #15962, #711, #24564, #5216, #7072, #13841, #3084, #20338, #16250, #995 ),
 ( #9583, #24293, #4941, #22176, #9303, #817, #18010, #15658, #4904, #9405, #22424, #26375, #26648, #3046, #26945, #17879, #7303, #26795, #13659, #15924, #13516, #20023, #4764, #24530, #5178, #13807, #11681, #24258, #16211, #7591, #22142, #20304, #17758, #961, #9548, #22012, #24665, #7036, #542, #16071, #9137, #18153, #7441, #5330, #2770, #13952, #9265, #22564, #2645, #9701, #26504, #3190, #11822, #11273, #20442, #7169, #1105, #19892, #15790, #18300, #27090, #8298, #8159, #20725, #22849, #18734 ) ),
 .UNSPECIFIED., .F., .T., .F.,
 ( 3, 3 ),
 ( 4, 2, 2, 2, 2, 2, 2, 2, 2, 2, 2, 2, 2, 2, 2, 2, 2, 2, 2, 2, 2, 2, 2, 2, 2, 2, 2, 2, 2, 2, 2, 2, 4 ),
 ( 0.000000000000000000, 1.000000000000000000 ),
 ( 0.000000000000000000, 0.1963495408493620697, 0.3926990816987241395, 0.5890486225480862092, 0.7853981633974482790, 0.9817477042468103487, 1.178097245096172418, 1.374446785945534488, 1.570796326794896558, 1.767145867644258628, 1.963495408493620697, 2.159844949342982545, 2.356194490192344837, 2.552544031041707129, 2.748893571891068976, 2.945243112740430824, 3.141592653589793116, 3.337942194439155408, 3.534291735288517255, 3.730641276137879103, 3.926990816987241395, 4.123340357836603687, 4.319689898685965090, 4.516039439535327382, 4.712388980384689674, 4.908738521234051966, 5.105088062083414258, 5.301437602932775661, 5.497787143782137953, 5.694136684631500245, 5.890486225480861648, 6.086835766330223940, 6.283185307179586232 ),
 .UNSPECIFIED. ) ;
#4411 = PLANE ( 'NONE',  #21842 ) ;
#4412 = EDGE_CURVE ( 'NONE', #16082, #27489, #1229, .T. ) ;
#4413 = AXIS2_PLACEMENT_3D ( 'NONE', #15060, #6843, #7242 ) ;
#4414 = ORIENTED_EDGE ( 'NONE', *, *, #5878, .F. ) ;
#4415 = ORIENTED_EDGE ( 'NONE', *, *, #10585, .F. ) ;
#4416 = ( REPRESENTATION_RELATIONSHIP ('NONE','NONE', #12434, #1615 ) REPRESENTATION_RELATIONSHIP_WITH_TRANSFORMATION ( #19337 )SHAPE_REPRESENTATION_RELATIONSHIP( ) ) ;
#4417 = EDGE_CURVE ( 'NONE', #10634, #5423, #18907, .T. ) ;
#4418 = EDGE_LOOP ( 'NONE', ( #6913, #20985, #27516, #4926 ) ) ;
#4419 = ADVANCED_FACE ( 'NONE', ( #15291, #8902 ), #6247, .T. ) ;
#4420 = CARTESIAN_POINT ( 'NONE',  ( 0.3121994997578272368, 0.4069448477569235778, -1.550196850393700920 ) ) ;
#4421 = DIRECTION ( 'NONE',  ( 1.000000000000000000, 0.000000000000000000, 0.000000000000000000 ) ) ;
#4422 = CARTESIAN_POINT ( 'NONE',  ( 0.1230388948667837656, -0.3365682031944939867, 0.1805249803472324666 ) ) ;
#4423 = EDGE_LOOP ( 'NONE', ( #3549, #11518, #17339, #23717, #25497, #2071, #23588, #11594, #16452, #3352, #5531, #4120, #96 ) ) ;
#4424 = CARTESIAN_POINT ( 'NONE',  ( -0.2564158049324432587, 0.4442166144912507164, -1.550196850393700920 ) ) ;
#4425 = DIRECTION ( 'NONE',  ( 0.9749279121818236193, -0.2225209339563147815, 0.000000000000000000 ) ) ;
#4426 = ORIENTED_EDGE ( 'NONE', *, *, #18669, .F. ) ;
#4427 = CARTESIAN_POINT ( 'NONE',  ( -0.2979095355689177493, -0.6203660015065670663, 0.1322834645669291320 ) ) ;
#4428 = AXIS2_PLACEMENT_3D ( 'NONE', #6355, #1687, #23175 ) ;
#4429 = CIRCLE ( 'NONE', #15696, 0.4267795243146149664 ) ;
#4430 = CARTESIAN_POINT ( 'NONE',  ( -0.6299212598425196763, 1.087444635826771533, -0.1051828227901515783 ) ) ;
#4431 = CARTESIAN_POINT ( 'NONE',  ( 0.3339160553493882300, 1.090203750159222551, -0.7502486126520099274 ) ) ;
#4432 = LINE ( 'NONE', #19684, #10993 ) ;
#4433 = ( GEOMETRIC_REPRESENTATION_CONTEXT ( 3 ) GLOBAL_UNCERTAINTY_ASSIGNED_CONTEXT ( ( #12136 ) ) GLOBAL_UNIT_ASSIGNED_CONTEXT ( ( #10314, #27571, #18788 ) ) REPRESENTATION_CONTEXT ( 'NONE', 'WORKASPACE' ) ) ;
#4434 = CARTESIAN_POINT ( 'NONE',  ( 0.03008364706454716778, -0.1136516277932334562, 0.1968503937007874127 ) ) ;
#4435 = FACE_OUTER_BOUND ( 'NONE', #1595, .T. ) ;
#4436 = EDGE_LOOP ( 'NONE', ( #7593, #13367, #19602, #25805 ) ) ;
#4437 = DIRECTION ( 'NONE',  ( 0.000000000000000000, -1.000000000000000000, 0.000000000000000000 ) ) ;
#4438 = DIRECTION ( 'NONE',  ( 0.000000000000000000, 1.000000000000000000, 0.000000000000000000 ) ) ;
#4439 = CARTESIAN_POINT ( 'NONE',  ( -0.03220957031754000111, 0.4921259842519685179, -1.550196850393700920 ) ) ;
#4440 = CARTESIAN_POINT ( 'NONE',  ( 0.3411003281197161341, 0.2991932138496539162, -1.934055118110236338 ) ) ;
#4441 = CIRCLE ( 'NONE', #14833, 0.6889763779527560139 ) ;
#4442 = CARTESIAN_POINT ( 'NONE',  ( 0.1643029338975805220, -0.4497088275977013661, 0.08349695147766536540 ) ) ;
#4443 = DIRECTION ( 'NONE',  ( 0.7660444431189777914, -0.6427876096865396960, 0.000000000000000000 ) ) ;
#4444 = CIRCLE ( 'NONE', #3510, 0.4803149606299212393 ) ;
#4445 = PRESENTATION_LAYER_ASSIGNMENT (  '', '', ( #17528 ) ) ;
#4446 = CARTESIAN_POINT ( 'NONE',  ( -0.0007595033562148819414, 0.6881885572739390167, 0.3401574803149606252 ) ) ;
#4447 = DIRECTION ( 'NONE',  ( 0.000000000000000000, 0.000000000000000000, 1.000000000000000000 ) ) ;
#4448 = EDGE_CURVE ( 'NONE', #5352, #13907, #21185, .T. ) ;
#4449 = DIRECTION ( 'NONE',  ( 0.000000000000000000, 1.000000000000000000, 0.000000000000000000 ) ) ;
#4450 = CARTESIAN_POINT ( 'NONE',  ( 0.2712695779737101520, 0.3534635626042424428, -1.934055118110236560 ) ) ;
#4451 = ORIENTED_EDGE ( 'NONE', *, *, #4099, .F. ) ;
#4452 = CARTESIAN_POINT ( 'NONE',  ( -0.7635713814939685262, 0.2990306848552756191, -0.1248922643827116152 ) ) ;
#4453 = ORIENTED_EDGE ( 'NONE', *, *, #16423, .F. ) ;
#4454 = CARTESIAN_POINT ( 'NONE',  ( 0.000000000000000000, 0.07874015748031495954, 0.000000000000000000 ) ) ;
#4455 = CARTESIAN_POINT ( 'NONE',  ( 0.1522836969735573143, -0.1970374587079578854, 0.4531137400369409374 ) ) ;
#4456 = CARTESIAN_POINT ( 'NONE',  ( 0.2249706821157846648, -0.9514344361775100012, -0.1680475531490076835 ) ) ;
#4457 = CARTESIAN_POINT ( 'NONE',  ( 0.000000000000000000, 0.1968503937007875237, 0.000000000000000000 ) ) ;
#4458 = AXIS2_PLACEMENT_3D ( 'NONE', #13653, #953, #22137 ) ;
#4459 = AXIS2_PLACEMENT_3D ( 'NONE', #23177, #16518, #18915 ) ;
#4460 = CARTESIAN_POINT ( 'NONE',  ( 0.4446020952038907681, 5.549066237130534971E-17, -1.934055118110236338 ) ) ;
#4461 = CARTESIAN_POINT ( 'NONE',  ( 0.2462256503455911016, 0.2807137536170354331, -3.115157480314960647 ) ) ;
#4462 = CIRCLE ( 'NONE', #20237, 0.2952755905264887182 ) ;
#4463 = CARTESIAN_POINT ( 'NONE',  ( -0.3661417322834645272, -0.4724409448818898127, -0.6411263657805729155 ) ) ;
#4464 = CARTESIAN_POINT ( 'NONE',  ( 0.4684132450478833976, -0.1062614382955264641, 0.2362204724409446843 ) ) ;
#4465 = EDGE_CURVE ( 'NONE', #24279, #12499, #12727, .T. ) ;
#4466 = VERTEX_POINT ( 'NONE', #15179 ) ;
#4467 = EDGE_CURVE ( 'NONE', #11052, #11455, #23463, .T. ) ;
#4468 = CARTESIAN_POINT ( 'NONE',  ( -0.6119360453657027854, 0.1072290460172413279, 0.2574803149606298969 ) ) ;
#4469 = ORIENTED_EDGE ( 'NONE', *, *, #3494, .F. ) ;
#4470 = AXIS2_PLACEMENT_3D ( 'NONE', #9684, #5310, #943 ) ;
#4471 = ADVANCED_FACE ( 'NONE', ( #4435 ), #21112, .T. ) ;
#4472 = ORIENTED_EDGE ( 'NONE', *, *, #8181, .F. ) ;
#4473 = CARTESIAN_POINT ( 'NONE',  ( -0.07217847769028858107, -4.927204724409449161E-18, 0.000000000000000000 ) ) ;
#4474 = VERTEX_POINT ( 'NONE', #8933 ) ;
#4475 = EDGE_CURVE ( 'NONE', #14551, #1582, #13040, .T. ) ;
#4476 = EDGE_LOOP ( 'NONE', ( #27104, #19325, #20943, #13965 ) ) ;
#4477 = CARTESIAN_POINT ( 'NONE',  ( 0.3874223757879868280, 0.3097832252409934428, 0.2989974301521946543 ) ) ;
#4478 = CARTESIAN_POINT ( 'NONE',  ( 0.3382184156732163660, 0.3855916753051394363, 1.766732283464566899 ) ) ;
#4479 = DIRECTION ( 'NONE',  ( 0.000000000000000000, 1.000000000000000000, 0.000000000000000000 ) ) ;
#4480 = CIRCLE ( 'NONE', #9406, 0.6751968503937006982 ) ;
#4481 = EDGE_LOOP ( 'NONE', ( #14759, #8403, #7371, #12289 ) ) ;
#4482 = ORIENTED_EDGE ( 'NONE', *, *, #5823, .T. ) ;
#4483 = AXIS2_PLACEMENT_3D ( 'NONE', #3323, #3468, #20296 ) ;
#4484 = CARTESIAN_POINT ( 'NONE',  ( 0.5510854067038989390, 0.4384931681285572647, 0.3281099440183985472 ) ) ;
#4485 = EDGE_LOOP ( 'NONE', ( #17552, #1995, #17553, #9444 ) ) ;
#4486 = AXIS2_PLACEMENT_3D ( 'NONE', #12309, #16278, #5540 ) ;
#4487 = ORIENTED_EDGE ( 'NONE', *, *, #3847, .F. ) ;
#4488 = DIRECTION ( 'NONE',  ( -0.9790454724845842893, -0.1018208755700880375, 0.1763589297585410332 ) ) ;
#4489 = CARTESIAN_POINT ( 'NONE',  ( 0.01504182353227358389, 0.000000000000000000, 0.000000000000000000 ) ) ;
#4490 = CARTESIAN_POINT ( 'NONE',  ( -0.2904160862623708650, 0.1677079028045392328, 1.953740157480315043 ) ) ;
#4491 = ORIENTED_EDGE ( 'NONE', *, *, #1366, .F. ) ;
#4492 = VERTEX_POINT ( 'NONE', #23928 ) ;
#4493 = DIRECTION ( 'NONE',  ( -0.000000000000000000, -0.000000000000000000, -1.000000000000000000 ) ) ;
#4494 = ORIENTED_EDGE ( 'NONE', *, *, #14386, .T. ) ;
#4495 = ORIENTED_EDGE ( 'NONE', *, *, #4565, .F. ) ;
#4496 = ORIENTED_EDGE ( 'NONE', *, *, #7820, .F. ) ;
#4497 = DIRECTION ( 'NONE',  ( 1.000000000000000000, 7.017815000000000124E-18, 0.000000000000000000 ) ) ;
#4498 = DIRECTION ( 'NONE',  ( -0.000000000000000000, -0.000000000000000000, 1.000000000000000000 ) ) ;
#4499 = CARTESIAN_POINT ( 'NONE',  ( -0.6299212598425196763, 0.000000000000000000, 0.000000000000000000 ) ) ;
#4500 = CARTESIAN_POINT ( 'NONE',  ( 0.7623981986069212624, 0.5947989165269446099, 0.09076627200198640610 ) ) ;
#4501 = VERTEX_POINT ( 'NONE', #21527 ) ;
#4502 = CONICAL_SURFACE ( 'NONE', #26570, 0.4863540308881693086, 1.365720138124999927 ) ;
#4503 = EDGE_CURVE ( 'NONE', #17070, #10201, #15405, .T. ) ;
#4504 = AXIS2_PLACEMENT_3D ( 'NONE', #21973, #13349, #4725 ) ;
#4505 = LINE ( 'NONE', #6767, #10977 ) ;
#4506 = EDGE_CURVE ( 'NONE', #12477, #26781, #2582, .T. ) ;
#4507 = EDGE_CURVE ( 'NONE', #3886, #11422, #11667, .T. ) ;
#4508 = DIRECTION ( 'NONE',  ( 0.000000000000000000, 0.000000000000000000, 1.000000000000000000 ) ) ;
#4509 = EDGE_CURVE ( 'NONE', #17836, #7391, #5385, .T. ) ;
#4510 = CARTESIAN_POINT ( 'NONE',  ( 0.000000000000000000, 0.000000000000000000, -0.2342519685039370358 ) ) ;
#4511 = FACE_OUTER_BOUND ( 'NONE', #20713, .T. ) ;
#4512 = CARTESIAN_POINT ( 'NONE',  ( -0.06880207798751733494, 0.1968503937007873850, -3.232982757847917554 ) ) ;
#4513 = VERTEX_POINT ( 'NONE', #19451 ) ;
#4514 = ORIENTED_EDGE ( 'NONE', *, *, #12938, .T. ) ;
#4515 = CYLINDRICAL_SURFACE ( 'NONE', #3724, 1.288838582677165556 ) ;
#4516 = ( CONVERSION_BASED_UNIT ( 'INCH', #17637 ) LENGTH_UNIT ( ) NAMED_UNIT ( #13045 ) ) ;
#4517 = DIRECTION ( 'NONE',  ( 0.000000000000000000, 0.000000000000000000, 1.000000000000000000 ) ) ;
#4518 = CIRCLE ( 'NONE', #9910, 0.1298643763538142593 ) ;
#4519 = ADVANCED_FACE ( 'NONE', ( #8848, #11110 ), #17337, .T. ) ;
#4520 = ORIENTED_EDGE ( 'NONE', *, *, #15404, .F. ) ;
#4521 = CARTESIAN_POINT ( 'NONE',  ( 0.000000000000000000, 0.000000000000000000, 1.953740157480315043 ) ) ;
#4522 = AXIS2_PLACEMENT_3D ( 'NONE', #23164, #4085, #12689 ) ;
#4523 = CARTESIAN_POINT ( 'NONE',  ( -0.6299212598425196763, 0.000000000000000000, 0.000000000000000000 ) ) ;
#4524 = PLANE ( 'NONE',  #26001 ) ;
#4525 = CARTESIAN_POINT ( 'NONE',  ( -0.4092566936344115835, 0.3255244810071337702, 0.1392975274210202508 ) ) ;
#4526 = VERTEX_POINT ( 'NONE', #17471 ) ;
#4527 = CARTESIAN_POINT ( 'NONE',  ( 0.1775991818008583745, 0.5230301363771922007, 0.9399606299212598381 ) ) ;
#4528 = CARTESIAN_POINT ( 'NONE',  ( -0.3937007873768824662, 4.821444090828918336E-17, -4.330708661417323135 ) ) ;
#4529 = ORIENTED_EDGE ( 'NONE', *, *, #13343, .F. ) ;
#4530 = CONICAL_SURFACE ( 'NONE', #18538, 0.4526932812344527379, 0.1178097243749990780 ) ;
#4531 = CARTESIAN_POINT ( 'NONE',  ( 0.2358179517464219221, 0.2802411498302517789, 0.08455817587866316931 ) ) ;
#4532 = DIRECTION ( 'NONE',  ( -0.9790454724845842893, -0.2036417511401760472, 2.493892000000000781E-17 ) ) ;
#4533 = CARTESIAN_POINT ( 'NONE',  ( 0.2979095355689177493, -0.6203660015065670663, 0.3401574803149606252 ) ) ;
#4534 = CARTESIAN_POINT ( 'NONE',  ( 0.1579154690111878589, -0.4355388305886193634, 0.1494804571160150142 ) ) ;
#4535 = DIRECTION ( 'NONE',  ( 0.000000000000000000, 0.000000000000000000, 1.000000000000000000 ) ) ;
#4536 = CARTESIAN_POINT ( 'NONE',  ( -0.0005056364805206488332, 0.3583524373864938606, 0.1805249803418977061 ) ) ;
#4537 = CARTESIAN_POINT ( 'NONE',  ( 0.5724622793732239145, -0.3313001865997644568, 0.1926811207713212126 ) ) ;
#4538 = CARTESIAN_POINT ( 'NONE',  ( 0.4173606904761050229, 5.111194336814911913E-17, -0.1464516454673935042 ) ) ;
#4539 = CARTESIAN_POINT ( 'NONE',  ( -0.2423050875943940918, 0.2890362931940642088, 0.07637549214372854611 ) ) ;
#4540 = DIRECTION ( 'NONE',  ( -1.000000000000000000, 0.000000000000000000, 0.000000000000000000 ) ) ;
#4541 = EDGE_CURVE ( 'NONE', #20920, #26710, #22131, .T. ) ;
#4542 = DIRECTION ( 'NONE',  ( 1.000000000000000000, 0.000000000000000000, 0.000000000000000000 ) ) ;
#4543 = FACE_OUTER_BOUND ( 'NONE', #439, .T. ) ;
#4544 = AXIS2_PLACEMENT_3D ( 'NONE', #19188, #21316, #8861 ) ;
#4545 = CARTESIAN_POINT ( 'NONE',  ( -0.4300830224589284878, -0.3772436174784035146, 0.9399606299212598381 ) ) ;
#4546 = DIRECTION ( 'NONE',  ( 0.000000000000000000, 0.000000000000000000, -1.000000000000000000 ) ) ;
#4547 = AXIS2_PLACEMENT_3D ( 'NONE', #5748, #14365, #23119 ) ;
#4548 = VERTEX_POINT ( 'NONE', #21443 ) ;
#4549 = ORIENTED_EDGE ( 'NONE', *, *, #1033, .F. ) ;
#4550 = CARTESIAN_POINT ( 'NONE',  ( -0.09139240964747710749, -0.07874015748031500117, -1.188614124534770567E-17 ) ) ;
#4551 = CARTESIAN_POINT ( 'NONE',  ( 0.4713455951423065060, -0.1082342125229984742, 0.2008762816149500807 ) ) ;
#4552 = VERTEX_POINT ( 'NONE', #2082 ) ;
#4553 = DIRECTION ( 'NONE',  ( 0.000000000000000000, 0.000000000000000000, 1.000000000000000000 ) ) ;
#4554 = ORIENTED_EDGE ( 'NONE', *, *, #10365, .T. ) ;
#4555 = ORIENTED_EDGE ( 'NONE', *, *, #16122, .T. ) ;
#4556 = AXIS2_PLACEMENT_3D ( 'NONE', #4457, #4048, #10531 ) ;
#4557 = DIRECTION ( 'NONE',  ( -0.2036417511401762415, -0.4895227362422910344, 0.8478782506317890100 ) ) ;
#4558 = CARTESIAN_POINT ( 'NONE',  ( 0.3988311005572732215, 0.4763376377695315300, 0.2574803149606298969 ) ) ;
#4559 = EDGE_CURVE ( 'NONE', #23196, #13737, #16668, .T. ) ;
#4560 = CARTESIAN_POINT ( 'NONE',  ( 0.000000000000000000, 0.4724409448818898127, 0.000000000000000000 ) ) ;
#4561 = CARTESIAN_POINT ( 'NONE',  ( 0.000000000000000000, 0.000000000000000000, 0.09685039370078740717 ) ) ;
#4562 = ORIENTED_EDGE ( 'NONE', *, *, #2324, .T. ) ;
#4563 = CARTESIAN_POINT ( 'NONE',  ( 0.06046064452055317090, 0.3092451502564478871, -3.626963221729183839 ) ) ;
#4564 = DIRECTION ( 'NONE',  ( -1.000000000000000000, 0.000000000000000000, 0.000000000000000000 ) ) ;
#4565 = EDGE_CURVE ( 'NONE', #19035, #26909, #23390, .T. ) ;
#4566 = CARTESIAN_POINT ( 'NONE',  ( 0.1477428134820237549, -0.4351030398461813720, -1.928289503579156294 ) ) ;
#4567 = CARTESIAN_POINT ( 'NONE',  ( -0.5511811023622047445, 0.000000000000000000, 0.9202755905511811330 ) ) ;
#4568 = APPLICATION_CONTEXT ( 'automotive_design' ) ;
#4569 = CARTESIAN_POINT ( 'NONE',  ( -0.6434710025615986151, -0.02921435793731240460, -0.2366737192061291462 ) ) ;
#4570 = FACE_OUTER_BOUND ( 'NONE', #17854, .T. ) ;
#4571 = CARTESIAN_POINT ( 'NONE',  ( -0.4714076450717705757, 0.08371568475171299595, 0.08349695147681061858 ) ) ;
#4572 = ORIENTED_EDGE ( 'NONE', *, *, #1208, .T. ) ;
#4573 = EDGE_CURVE ( 'NONE', #16402, #11118, #26557, .T. ) ;
#4574 = CIRCLE ( 'NONE', #17640, 0.5511811023268710086 ) ;
#4575 = CARTESIAN_POINT ( 'NONE',  ( 0.000000000000000000, 0.000000000000000000, 0.1322834645669291320 ) ) ;
#4576 = CARTESIAN_POINT ( 'NONE',  ( 0.3680051700917441604, 0.000000000000000000, 0.000000000000000000 ) ) ;
#4577 = ORIENTED_EDGE ( 'NONE', *, *, #21640, .F. ) ;
#4578 = PLANE ( 'NONE',  #10029 ) ;
#4579 = LINE ( 'NONE', #17578, #6039 ) ;
#4580 = CARTESIAN_POINT ( 'NONE',  ( -0.6996199877990079141, 0.1591959485999228652, 0.2265176967194976465 ) ) ;
#4581 = EDGE_LOOP ( 'NONE', ( #20664, #22877 ) ) ;
#4582 = CARTESIAN_POINT ( 'NONE',  ( -0.05926487674658593302, 0.4498374011143062567, -1.934055118110236338 ) ) ;
#4583 = DIRECTION ( 'NONE',  ( 0.000000000000000000, 0.000000000000000000, -1.000000000000000000 ) ) ;
#4584 = DIRECTION ( 'NONE',  ( 0.000000000000000000, 1.000000000000000000, 0.000000000000000000 ) ) ;
#4585 = CARTESIAN_POINT ( 'NONE',  ( -0.3992017438595018564, -0.2298214351608254269, 0.1771653543307087630 ) ) ;
#4586 = CARTESIAN_POINT ( 'NONE',  ( -0.7874015748031496509, 0.6226544199590670070, -0.5245967315940827103 ) ) ;
#4587 = CARTESIAN_POINT ( 'NONE',  ( 0.000000000000000000, 0.5322834645669292097, 0.4724409448818898127 ) ) ;
#4588 = DIRECTION ( 'NONE',  ( -0.000000000000000000, 1.000000000000000000, -0.000000000000000000 ) ) ;
#4589 = DIRECTION ( 'NONE',  ( 0.000000000000000000, -1.000000000000000000, 0.000000000000000000 ) ) ;
#4590 = CARTESIAN_POINT ( 'NONE',  ( -0.2602238532265429005, 0.000000000000000000, 0.2362204724409449064 ) ) ;
#4591 = EDGE_CURVE ( 'NONE', #14336, #3819, #14026, .T. ) ;
#4592 = VERTEX_POINT ( 'NONE', #13879 ) ;
#4593 = CARTESIAN_POINT ( 'NONE',  ( -0.06441914069860958658, -0.4921259842519685179, -1.569881889763779403 ) ) ;
#4594 = ORIENTED_EDGE ( 'NONE', *, *, #14859, .T. ) ;
#4595 = ORIENTED_EDGE ( 'NONE', *, *, #25777, .T. ) ;
#4596 = PLANE ( 'NONE',  #1133 ) ;
#4597 = LINE ( 'NONE', #9107, #6365 ) ;
#4598 = CARTESIAN_POINT ( 'NONE',  ( 0.2268096725222374654, 0.4600326175560591202, 1.766732283464566899 ) ) ;
#4599 = DIRECTION ( 'NONE',  ( 1.000000000000000000, 0.000000000000000000, 0.000000000000000000 ) ) ;
#4600 = VECTOR ( 'NONE', #27809, 39.37007874015748854 ) ;
#4601 = EDGE_LOOP ( 'NONE', ( #8593, #488, #3966, #15163 ) ) ;
#4602 = AXIS2_PLACEMENT_3D ( 'NONE', #20757, #18330, #16510 ) ;
#4603 = ORIENTED_EDGE ( 'NONE', *, *, #19074, .F. ) ;
#4604 = CARTESIAN_POINT ( 'NONE',  ( 0.3535721684718142188, -0.1200583359873150652, -3.115157480314960647 ) ) ;
#4605 = VERTEX_POINT ( 'NONE', #20234 ) ;
#4606 = DIRECTION ( 'NONE',  ( 0.000000000000000000, 0.000000000000000000, 1.000000000000000000 ) ) ;
#4607 = CARTESIAN_POINT ( 'NONE',  ( 0.1522836969735573143, 0.2938892803217901806, -0.3971963147566898167 ) ) ;
#4608 = ORIENTED_EDGE ( 'NONE', *, *, #25493, .T. ) ;
#4609 = ADVANCED_FACE ( 'NONE', ( #24602 ), #24890, .T. ) ;
#4610 = ORIENTED_EDGE ( 'NONE', *, *, #17812, .F. ) ;
#4611 = VECTOR ( 'NONE', #3907, 39.37007874015748143 ) ;
#4612 = SHAPE_REPRESENTATION ( 'Index Plate', ( #11588 ), #8455 ) ;
#4613 = CARTESIAN_POINT ( 'NONE',  ( 0.3268074212154850611, -0.1882834141668342509, 0.1992142436757342316 ) ) ;
#4614 = FACE_OUTER_BOUND ( 'NONE', #15635, .T. ) ;
#4615 = ORIENTED_EDGE ( 'NONE', *, *, #5314, .T. ) ;
#4616 = B_SPLINE_CURVE_WITH_KNOTS ( 'NONE', 3,
 ( #12687, #12828, #21461, #6761, #2099, #19327 ),
 .UNSPECIFIED., .F., .F.,
 ( 4, 1, 1, 4 ),
 ( 0.000000000000000000, 0.2857142857142853098, 0.5714285714285706197, 1.000000000000000000 ),
 .UNSPECIFIED. ) ;
#4617 = ORIENTED_EDGE ( 'NONE', *, *, #15636, .T. ) ;
#4618 = VERTEX_POINT ( 'NONE', #22357 ) ;
#4619 = DIRECTION ( 'NONE',  ( -0.2225209339563143096, 0.9749279121818235083, 0.000000000000000000 ) ) ;
#4620 = ADVANCED_FACE ( 'NONE', ( #13735 ), #14309, .T. ) ;
#4621 = CARTESIAN_POINT ( 'NONE',  ( 0.4245040230929275626, 0.9715221028222027488, -0.4707374946848913444 ) ) ;
#4622 = DIRECTION ( 'NONE',  ( -1.000000000000000000, 0.000000000000000000, 0.000000000000000000 ) ) ;
#4623 = CARTESIAN_POINT ( 'NONE',  ( -0.07874015748031495954, -0.04546065111729338803, -0.4724409448818898127 ) ) ;
#4624 = ORIENTED_EDGE ( 'NONE', *, *, #6538, .F. ) ;
#4625 = PRODUCT_DEFINITION_SHAPE ( 'NONE', 'NONE',  #27902 ) ;
#4626 = VECTOR ( 'NONE', #24210, 39.37007874015748143 ) ;
#4627 = CYLINDRICAL_SURFACE ( 'NONE', #17309, 0.5322834645669292097 ) ;
#4628 = FACE_OUTER_BOUND ( 'NONE', #20418, .T. ) ;
#4629 = AXIS2_PLACEMENT_3D ( 'NONE', #11749, #5251, #25164 ) ;
#4630 = LINE ( 'NONE', #11409, #27280 ) ;
#4631 = FACE_OUTER_BOUND ( 'NONE', #27267, .T. ) ;
#4632 = FILL_AREA_STYLE ('',( #11005 ) ) ;
#4633 = EDGE_CURVE ( 'NONE', #16172, #8069, #14422, .T. ) ;
#4634 = DIRECTION ( 'NONE',  ( 0.000000000000000000, 0.000000000000000000, 1.000000000000000000 ) ) ;
#4635 = EDGE_LOOP ( 'NONE', ( #142, #12752 ) ) ;
#4636 = ORIENTED_EDGE ( 'NONE', *, *, #16319, .T. ) ;
#4637 = CARTESIAN_POINT ( 'NONE',  ( 0.3916295560431587996, 0.3131429078201153904, 0.1643955689120278618 ) ) ;
#4638 = LENGTH_MEASURE_WITH_UNIT ( LENGTH_MEASURE( 0.02539999999999999897 ), #11144 ) ;
#4639 = CARTESIAN_POINT ( 'NONE',  ( 0.2341095169845144042, -0.2669917830071620313, 1.953740157480315043 ) ) ;
#4640 = VECTOR ( 'NONE', #11392, 39.37007874015748143 ) ;
#4641 = ORIENTED_EDGE ( 'NONE', *, *, #23, .T. ) ;
#4642 = CARTESIAN_POINT ( 'NONE',  ( 0.6751968503937006982, 8.353151887884997269E-17, -0.2755905511811023723 ) ) ;
#4643 = VECTOR ( 'NONE', #21062, 39.37007874015748143 ) ;
#4644 = FACE_OUTER_BOUND ( 'NONE', #18336, .T. ) ;
#4645 = CARTESIAN_POINT ( 'NONE',  ( 0.6707652279343464530, -0.1538768215239712522, 0.1322834645669291320 ) ) ;
#4646 = DIRECTION ( 'NONE',  ( 0.9848077530122082424, 0.1736481776669299149, -0.000000000000000000 ) ) ;
#4647 = ORIENTED_EDGE ( 'NONE', *, *, #24298, .T. ) ;
#4648 = CARTESIAN_POINT ( 'NONE',  ( -0.03607471876262562105, -0.5511811023622046335, 0.9202755905511811330 ) ) ;
#4649 = VERTEX_POINT ( 'NONE', #20650 ) ;
#4650 = EDGE_CURVE ( 'NONE', #2222, #5851, #10328, .T. ) ;
#4651 = CARTESIAN_POINT ( 'NONE',  ( -0.4980314960629921295, 0.000000000000000000, -0.01377952755905511792 ) ) ;
#4652 = ORIENTED_EDGE ( 'NONE', *, *, #5150, .T. ) ;
#4653 = AXIS2_PLACEMENT_3D ( 'NONE', #8465, #16949, #17084 ) ;
#4654 = CARTESIAN_POINT ( 'NONE',  ( 0.2230788859036007821, 0.2650812153444456198, 0.1377952755905513527 ) ) ;
#4655 = EDGE_CURVE ( 'NONE', #25431, #17836, #23895, .T. ) ;
#4656 = CARTESIAN_POINT ( 'NONE',  ( 0.3012109481302311376, 0.3598698725862007897, 0.07637795275590551769 ) ) ;
#4657 = AXIS2_PLACEMENT_3D ( 'NONE', #23628, #21498, #4264 ) ;
#4658 = DIRECTION ( 'NONE',  ( 0.000000000000000000, 0.000000000000000000, -1.000000000000000000 ) ) ;
#4659 = LINE ( 'NONE', #15145, #3219 ) ;
#4660 = CARTESIAN_POINT ( 'NONE',  ( 0.3204319178469888230, -0.6672004808833374989, 0.2161412452789004401 ) ) ;
#4661 = DIRECTION ( 'NONE',  ( -1.000000000000000000, 0.000000000000000000, 0.000000000000000000 ) ) ;
#4662 = DIRECTION ( 'NONE',  ( 0.000000000000000000, 0.000000000000000000, 1.000000000000000000 ) ) ;
#4663 = B_SPLINE_CURVE_WITH_KNOTS ( 'NONE', 3,
 ( #16020, #20111, #12056, #20675, #769, #9358 ),
 .UNSPECIFIED., .F., .F.,
 ( 4, 2, 4 ),
 ( 0.3000437156586439613, 0.3015484798814579981, 0.3030532441042709801 ),
 .UNSPECIFIED. ) ;
#4664 = AXIS2_PLACEMENT_3D ( 'NONE', #17436, #24211, #26057 ) ;
#4665 = VECTOR ( 'NONE', #13639, 39.37007874015748854 ) ;
#4666 = CARTESIAN_POINT ( 'NONE',  ( 0.2860899518037664513, 0.4954156765914491944, 0.9399606299212598381 ) ) ;
#4667 = DIRECTION ( 'NONE',  ( 0.000000000000000000, 0.000000000000000000, 1.000000000000000000 ) ) ;
#4668 = FACE_OUTER_BOUND ( 'NONE', #11145, .T. ) ;
#4669 = VECTOR ( 'NONE', #6048, 39.37007874015748143 ) ;
#4670 = ORIENTED_EDGE ( 'NONE', *, *, #25230, .T. ) ;
#4671 = CIRCLE ( 'NONE', #19590, 1.131889763779527547 ) ;
#4672 = ORIENTED_EDGE ( 'NONE', *, *, #20993, .F. ) ;
#4673 = EDGE_CURVE ( 'NONE', #25416, #22409, #21629, .T. ) ;
#4674 = CARTESIAN_POINT ( 'NONE',  ( -0.1327036767636080028, -0.4954415918535519658, -1.550196850393700920 ) ) ;
#4675 = DIRECTION ( 'NONE',  ( 0.000000000000000000, 0.000000000000000000, -1.000000000000000000 ) ) ;
#4676 = PLANE ( 'NONE',  #18658 ) ;
#4677 = CYLINDRICAL_SURFACE ( 'NONE', #19084, 0.1308464566929133932 ) ;
#4678 = ORIENTED_EDGE ( 'NONE', *, *, #6857, .T. ) ;
#4679 = EDGE_CURVE ( 'NONE', #14162, #3630, #27583, .T. ) ;
#4680 = AXIS2_PLACEMENT_3D ( 'NONE', #26546, #2807, #9308 ) ;
#4681 = FACE_OUTER_BOUND ( 'NONE', #8261, .T. ) ;
#4682 = CARTESIAN_POINT ( 'NONE',  ( 0.5511811023622047445, 0.000000000000000000, -1.550196850393700920 ) ) ;
#4683 = CARTESIAN_POINT ( 'NONE',  ( 0.000000000000000000, 0.000000000000000000, 0.1377952755905511861 ) ) ;
#4684 = CARTESIAN_POINT ( 'NONE',  ( 0.3339160553493882300, 0.9384519710407874804, -0.7923371756411300426 ) ) ;
#4685 = CARTESIAN_POINT ( 'NONE',  ( -0.5525004126151165096, 0.09742072959660473541, 0.1771653543307086520 ) ) ;
#4686 = AXIS2_PLACEMENT_3D ( 'NONE', #10403, #2980, #24200 ) ;
#4687 = CARTESIAN_POINT ( 'NONE',  ( 0.000000000000000000, 0.000000000000000000, -0.4724409448841456749 ) ) ;
#4688 = AXIS2_PLACEMENT_3D ( 'NONE', #8241, #10061, #18815 ) ;
#4689 = ORIENTED_EDGE ( 'NONE', *, *, #1718, .T. ) ;
#4690 = DIRECTION ( 'NONE',  ( -0.8660254037844382635, -0.5000000000000005551, 0.000000000000000000 ) ) ;
#4691 = DIRECTION ( 'NONE',  ( 0.000000000000000000, 0.000000000000000000, -1.000000000000000000 ) ) ;
#4692 = CARTESIAN_POINT ( 'NONE',  ( -0.4585215200179055817, 0.000000000000000000, -1.928289503579156516 ) ) ;
#4693 = ORIENTED_EDGE ( 'NONE', *, *, #25354, .F. ) ;
#4694 = CARTESIAN_POINT ( 'NONE',  ( 0.3645739570812638330, -0.2796934465393868807, -1.928289503579156072 ) ) ;
#4695 = LINE ( 'NONE', #15721, #11225 ) ;
#4696 = CARTESIAN_POINT ( 'NONE',  ( -0.5791695622062364990, 0.4608640948057729503, 0.2562996995975141967 ) ) ;
#4697 = CARTESIAN_POINT ( 'NONE',  ( -0.06001958459474868862, 0.4555658499976078524, -1.928289503579158515 ) ) ;
#4698 = VECTOR ( 'NONE', #25982, 39.37007874015748143 ) ;
#4699 = CARTESIAN_POINT ( 'NONE',  ( 3.644242538420618632E-18, 0.5007874015748032814, 0.09684793308443545579 ) ) ;
#4700 = SPHERICAL_SURFACE ( 'NONE', #5819, 0.1003956692913385851 ) ;
#4701 = CARTESIAN_POINT ( 'NONE',  ( -0.6112138326843681302, -0.1217116465605828785, -0.08634548179755788255 ) ) ;
#4702 = CARTESIAN_POINT ( 'NONE',  ( 0.000000000000000000, 0.000000000000000000, 0.1377952755905511861 ) ) ;
#4703 = CARTESIAN_POINT ( 'NONE',  ( -6.518592411209533944E-17, -0.5322834645669292097, -1.092739370078740131E-17 ) ) ;
#4704 = ORIENTED_EDGE ( 'NONE', *, *, #272, .F. ) ;
#4706 = ADVANCED_FACE ( 'NONE', ( #11033 ), #15154, .T. ) ;
#4705 = CIRCLE ( 'NONE', #24121, 0.7539370078740157410 ) ;
#4707 = DIRECTION ( 'NONE',  ( 0.8660254037844385966, -0.5000000000000000000, 0.000000000000000000 ) ) ;
#4708 = EDGE_CURVE ( 'NONE', #22917, #18857, #12599, .T. ) ;
#4709 = FACE_OUTER_BOUND ( 'NONE', #18885, .T. ) ;
#4710 = AXIS2_PLACEMENT_3D ( 'NONE', #8153, #20999, #16762 ) ;
#4711 = FACE_OUTER_BOUND ( 'NONE', #27003, .T. ) ;
#4712 = CARTESIAN_POINT ( 'NONE',  ( 2.664928230027803213, -0.4724409448818898127, 0.9265594366467145848 ) ) ;
#4713 = ADVANCED_FACE ( 'NONE', ( #21219 ), #23418, .T. ) ;
#4714 = DIRECTION ( 'NONE',  ( 0.000000000000000000, 0.000000000000000000, -1.000000000000000000 ) ) ;
#4715 = CARTESIAN_POINT ( 'NONE',  ( -0.7121770198535963825, 0.1302456093167436990, -0.2464793285356193242 ) ) ;
#4716 = ORIENTED_EDGE ( 'NONE', *, *, #16150, .F. ) ;
#4717 = CARTESIAN_POINT ( 'NONE',  ( 0.4980314960629921295, 6.099126775281109802E-17, -0.2618110236220472231 ) ) ;
#4718 = FACE_OUTER_BOUND ( 'NONE', #9689, .T. ) ;
#4719 = AXIS2_PLACEMENT_3D ( 'NONE', #7600, #9709, #5622 ) ;
#4720 = CARTESIAN_POINT ( 'NONE',  ( -0.2262947209311158003, -0.4714317853986079720, 0.3331434174507413304 ) ) ;
#4721 = EDGE_CURVE ( 'NONE', #15921, #17206, #826, .T. ) ;
#4722 = CARTESIAN_POINT ( 'NONE',  ( 0.3572819248074444731, 0.1213180142433879782, -3.100567304031760951 ) ) ;
#4723 = CARTESIAN_POINT ( 'NONE',  ( 0.3680051700917441604, 0.000000000000000000, 0.000000000000000000 ) ) ;
#4724 = DIRECTION ( 'NONE',  ( 0.000000000000000000, 0.000000000000000000, -1.000000000000000000 ) ) ;
#4725 = DIRECTION ( 'NONE',  ( 0.000000000000000000, 0.000000000000000000, 1.000000000000000000 ) ) ;
#4726 = ADVANCED_FACE ( 'NONE', ( #4125 ), #13008, .F. ) ;
#4727 = EDGE_LOOP ( 'NONE', ( #14075, #24927 ) ) ;
#4728 = LINE ( 'NONE', #2474, #26272 ) ;
#4729 = AXIS2_PLACEMENT_3D ( 'NONE', #14420, #9581, #12972 ) ;
#4730 = ORIENTED_EDGE ( 'NONE', *, *, #20377, .F. ) ;
#4731 = ORIENTED_EDGE ( 'NONE', *, *, #2278, .T. ) ;
#4732 = CARTESIAN_POINT ( 'NONE',  ( -6.518592411209533944E-17, -0.5322834645669292097, 0.4062992125984251635 ) ) ;
#4733 = CARTESIAN_POINT ( 'NONE',  ( 0.000000000000000000, 0.000000000000000000, 0.1992125984251968684 ) ) ;
#4734 = APPLICATION_PROTOCOL_DEFINITION ( 'draft international standard', 'automotive_design', 1998, #22809 ) ;
#4735 = CARTESIAN_POINT ( 'NONE',  ( -0.1649135259617106886, 0.4856708409200803378, 1.747047244094488194 ) ) ;
#4736 = CIRCLE ( 'NONE', #16024, 0.1299232283464567539 ) ;
#4737 = CARTESIAN_POINT ( 'NONE',  ( -0.3214446924536846772, 0.3840069416942866742, 0.2574803149606298969 ) ) ;
#4738 = ORIENTED_EDGE ( 'NONE', *, *, #17439, .F. ) ;
#4739 = VERTEX_POINT ( 'NONE', #19510 ) ;
#4741 = CARTESIAN_POINT ( 'NONE',  ( -0.2462256503456003442, -0.2807137536170363767, -3.115157480314960647 ) ) ;
#4740 = CARTESIAN_POINT ( 'NONE',  ( 0.5385210225480960844, 0.4284847435812472183, 0.3401574803149606252 ) ) ;
#4742 = LINE ( 'NONE', #148, #10499 ) ;
#4743 = CARTESIAN_POINT ( 'NONE',  ( 0.000000000000000000, 0.000000000000000000, -0.006889763779527558960 ) ) ;
#4744 = EDGE_CURVE ( 'NONE', #23791, #26519, #25173, .T. ) ;
#4745 = CARTESIAN_POINT ( 'NONE',  ( -0.2211428102655801364, -0.2521176338356625468, 1.953740157480315043 ) ) ;
#4746 = EDGE_LOOP ( 'NONE', ( #8223, #13844, #16495, #15110 ) ) ;
#4747 = ORIENTED_EDGE ( 'NONE', *, *, #3170, .F. ) ;
#4748 = CIRCLE ( 'NONE', #1588, 0.3464566929133857665 ) ;
#4749 = ADVANCED_FACE ( 'NONE', ( #328 ), #25632, .F. ) ;
#4750 = DIRECTION ( 'NONE',  ( 0.000000000000000000, 0.000000000000000000, 1.000000000000000000 ) ) ;
#4751 = CIRCLE ( 'NONE', #16056, 0.8267716535433071723 ) ;
#4752 = VERTEX_POINT ( 'NONE', #15014 ) ;
#4753 = ORIENTED_EDGE ( 'NONE', *, *, #15365, .F. ) ;
#4754 = VERTEX_POINT ( 'NONE', #19373 ) ;
#4755 = CARTESIAN_POINT ( 'NONE',  ( -0.03962986251637951735, 0.1968503937007874127, -3.617043892030582963 ) ) ;
#4756 = AXIS2_PLACEMENT_3D ( 'NONE', #19564, #6847, #15065 ) ;
#4757 = CARTESIAN_POINT ( 'NONE',  ( 9.642888182262624280E-17, 0.4724409448818898127, 0.7874015748031496509 ) ) ;
#4758 = DIRECTION ( 'NONE',  ( -1.000000000000000000, 0.000000000000000000, 0.000000000000000000 ) ) ;
#4759 = CARTESIAN_POINT ( 'NONE',  ( 0.7874015748031496509, 0.4724409448818898127, 0.000000000000000000 ) ) ;
#4760 = ORIENTED_EDGE ( 'NONE', *, *, #9446, .F. ) ;
#4761 = CIRCLE ( 'NONE', #2067, 0.1110236220424516002 ) ;
#4762 = CARTESIAN_POINT ( 'NONE',  ( 0.1504127680535784495, -0.2090906986543966672, -0.4378338296930543438 ) ) ;
#4763 = CARTESIAN_POINT ( 'NONE',  ( -0.5393700787401575214, 6.605378404849898113E-17, 0.01181102362204724393 ) ) ;
#4764 = CARTESIAN_POINT ( 'NONE',  ( -0.1775730735577547292, 0.3074993854542629190, 1.953740157480315043 ) ) ;
#4765 = CARTESIAN_POINT ( 'NONE',  ( -0.0006679551606482677165, 0.5322830454629158270, 0.3401574803149606252 ) ) ;
#4766 = EDGE_CURVE ( 'NONE', #21315, #23520, #2608, .T. ) ;
#4767 = FACE_OUTER_BOUND ( 'NONE', #8375, .T. ) ;
#4768 = AXIS2_PLACEMENT_3D ( 'NONE', #13400, #21895, #435 ) ;
#4769 = DIRECTION ( 'NONE',  ( 0.000000000000000000, 0.000000000000000000, 1.000000000000000000 ) ) ;
#4770 = CARTESIAN_POINT ( 'NONE',  ( -2.685748425196850164E-17, 0.000000000000000000, -3.745078740157480546 ) ) ;
#4771 = CARTESIAN_POINT ( 'NONE',  ( -0.03349795313264326141, 0.5118110236220472231, 1.766732283464566899 ) ) ;
#4772 = CIRCLE ( 'NONE', #12909, 0.4226968503937005295 ) ;
#4773 = VERTEX_POINT ( 'NONE', #6251 ) ;
#4774 = CARTESIAN_POINT ( 'NONE',  ( 0.4302903874092360303, -0.2491168502850711342, 0.1615162260879781098 ) ) ;
#4775 = ORIENTED_EDGE ( 'NONE', *, *, #23661, .F. ) ;
#4776 = ADVANCED_FACE ( 'NONE', ( #70 ), #12569, .T. ) ;
#4777 = DIRECTION ( 'NONE',  ( 0.000000000000000000, -1.000000000000000000, 0.000000000000000000 ) ) ;
#4778 = ORIENTED_EDGE ( 'NONE', *, *, #18833, .T. ) ;
#4779 = CARTESIAN_POINT ( 'NONE',  ( -0.4622619257814346572, 0.08092139668567638333, 0.07637795275590551769 ) ) ;
#4780 = CARTESIAN_POINT ( 'NONE',  ( -0.4921259842519685179, 0.03220957031763950484, -1.569881889763779625 ) ) ;
#4781 = LINE ( 'NONE', #15419, #1205 ) ;
#4782 = ORIENTED_EDGE ( 'NONE', *, *, #16080, .T. ) ;
#4783 = CARTESIAN_POINT ( 'NONE',  ( 0.1775991818008606782, -0.5230301363771325818, 0.9202755905511811330 ) ) ;
#4784 = ORIENTED_EDGE ( 'NONE', *, *, #5227, .F. ) ;
#4785 = CARTESIAN_POINT ( 'NONE',  ( 0.1287090038540879555, -0.1704774416898497957, 0.09842519685039353983 ) ) ;
#4786 = EDGE_LOOP ( 'NONE', ( #13307, #18454, #15039, #24615 ) ) ;
#4787 = CARTESIAN_POINT ( 'NONE',  ( -0.1285103288269285327, -0.3545966721392122545, 0.07637795275590551769 ) ) ;
#4788 = CIRCLE ( 'NONE', #19221, 0.3771653543307086909 ) ;
#4789 = DIRECTION ( 'NONE',  ( -0.000000000000000000, -1.000000000000000000, -0.000000000000000000 ) ) ;
#4790 = CARTESIAN_POINT ( 'NONE',  ( -0.3872945158171015589, 0.000000000000000000, -0.2342519685039370358 ) ) ;
#4791 = CARTESIAN_POINT ( 'NONE',  ( -2.685748425196850164E-17, 0.000000000000000000, -3.115157480314960647 ) ) ;
#4792 = CARTESIAN_POINT ( 'NONE',  ( 0.3105958729525251649, -0.6467467715319020760, 0.1601585119471421181 ) ) ;
#4793 = DIRECTION ( 'NONE',  ( 1.000000000000000000, 0.000000000000000000, 0.000000000000000000 ) ) ;
#4794 = CARTESIAN_POINT ( 'NONE',  ( 0.1279527559055118058, 0.7874015748031496509, 0.000000000000000000 ) ) ;
#4795 = VERTEX_POINT ( 'NONE', #8631 ) ;
#4796 = EDGE_CURVE ( 'NONE', #19119, #20886, #12731, .T. ) ;
#4797 = DIRECTION ( 'NONE',  ( 0.000000000000000000, 0.000000000000000000, -1.000000000000000000 ) ) ;
#4798 = EDGE_CURVE ( 'NONE', #25818, #23475, #22481, .T. ) ;
#4799 = CARTESIAN_POINT ( 'NONE',  ( -0.3200513472070305454, 0.3804946224880222383, 0.1615162260920062487 ) ) ;
#4800 = DIRECTION ( 'NONE',  ( -1.000000000000000000, 0.000000000000000000, 0.000000000000000000 ) ) ;
#4801 = DIRECTION ( 'NONE',  ( 0.000000000000000000, -1.000000000000000000, 0.000000000000000000 ) ) ;
#4802 = CARTESIAN_POINT ( 'NONE',  ( 0.5131133041954023533, 0.2529800193559384458, 0.9399606299212598381 ) ) ;
#4803 = CARTESIAN_POINT ( 'NONE',  ( 0.2303471512294322787, -0.4798602677570401598, 0.3401574803149606252 ) ) ;
#4804 = PRODUCT_RELATED_PRODUCT_CATEGORY ( 'part', '', ( #25356 ) ) ;
#4805 = VERTEX_POINT ( 'NONE', #21773 ) ;
#4806 = CARTESIAN_POINT ( 'NONE',  ( 0.000000000000000000, 0.000000000000000000, 0.07637795275590551769 ) ) ;
#4807 = ADVANCED_FACE ( 'NONE', ( #17392 ), #18382, .T. ) ;
#4808 = EDGE_CURVE ( 'NONE', #23881, #14114, #4444, .T. ) ;
#4809 = AXIS2_PLACEMENT_3D ( 'NONE', #17963, #24618, #5276 ) ;
#4810 = EDGE_CURVE ( 'NONE', #10058, #27798, #16685, .T. ) ;
#4811 = VERTEX_POINT ( 'NONE', #7588 ) ;
#4812 = CIRCLE ( 'NONE', #22864, 0.3937007874015748254 ) ;
#4813 = CYLINDRICAL_SURFACE ( 'NONE', #23754, 0.4842519685039370358 ) ;
#4814 = CARTESIAN_POINT ( 'NONE',  ( 0.1516263115863346334, -0.1971492568089275588, -0.4530651079966787620 ) ) ;
#4815 = ORIENTED_EDGE ( 'NONE', *, *, #20578, .T. ) ;
#4816 = B_SPLINE_CURVE_WITH_KNOTS ( 'NONE', 3,
 ( #27616, #452, #8258, #4022 ),
 .UNSPECIFIED., .F., .F.,
 ( 4, 4 ),
 ( 0.000000000000000000, 1.000000000000000000 ),
 .UNSPECIFIED. ) ;
#4817 = CARTESIAN_POINT ( 'NONE',  ( -0.5905511811023621549, 0.000000000000000000, 0.000000000000000000 ) ) ;
#4818 = PLANE ( 'NONE',  #10795 ) ;
#4819 = CARTESIAN_POINT ( 'NONE',  ( -0.4537304931026617250, 0.07942646906834203990, 0.1639447408816315788 ) ) ;
#4820 = CARTESIAN_POINT ( 'NONE',  ( 0.5309636003393858328, 0.8781547594069606388, -0.3365259449620598975 ) ) ;
#4821 = CARTESIAN_POINT ( 'NONE',  ( 0.000000000000000000, 0.000000000000000000, 0.3425196850393700809 ) ) ;
#4822 = ( BOUNDED_CURVE ( )  B_SPLINE_CURVE ( 2, ( #2699, #15333, #6692 ),
 .UNSPECIFIED., .F., .T. ) 
 B_SPLINE_CURVE_WITH_KNOTS ( ( 3, 3 ),
 ( 0.000000000000000000, 0.2336872276155829986 ),
 .UNSPECIFIED. ) 
 CURVE ( )  GEOMETRIC_REPRESENTATION_ITEM ( )  RATIONAL_B_SPLINE_CURVE ( ( 1.000000000000000000, 1.154700538379245911, 1.000000000000000000 ) ) 
 REPRESENTATION_ITEM ( '' )  ) ;
#4823 = EDGE_CURVE ( 'NONE', #11214, #23414, #20724, .T. ) ;
#4824 = CARTESIAN_POINT ( 'NONE',  ( -0.04956879728060041568, 0.2165354330708661457, -3.634230943735655472 ) ) ;
#4825 = CARTESIAN_POINT ( 'NONE',  ( 0.07874015748031495954, 0.04546065111729338803, -0.3779527559055118058 ) ) ;
#4826 = B_SPLINE_CURVE_WITH_KNOTS ( 'NONE', 3,
 ( #25756, #21789, #15034, #6681, #8785, #15173 ),
 .UNSPECIFIED., .F., .F.,
 ( 4, 2, 4 ),
 ( 0.000000000000000000, 0.2500000000000000000, 0.5000000000000000000 ),
 .UNSPECIFIED. ) ;
#4827 = ORIENTED_EDGE ( 'NONE', *, *, #21054, .F. ) ;
#4828 = CARTESIAN_POINT ( 'NONE',  ( -1.452994488188976472E-16, 0.3149606299212598381, -3.646653543307086576 ) ) ;
#4829 = CARTESIAN_POINT ( 'NONE',  ( 0.2268096725200263730, 0.4600326175569572351, -1.550196850393700920 ) ) ;
#4830 = EDGE_CURVE ( 'NONE', #6451, #14713, #16029, .T. ) ;
#4831 = CARTESIAN_POINT ( 'NONE',  ( -0.03001016326913591784, 0.4585215200179055817, -1.928289503579156516 ) ) ;
#4832 = AXIS2_PLACEMENT_3D ( 'NONE', #8544, #25638, #106 ) ;
#4833 = DIRECTION ( 'NONE',  ( 1.000000000000000000, 0.000000000000000000, 0.000000000000000000 ) ) ;
#4834 = FACE_BOUND ( 'NONE', #5849, .T. ) ;
#4835 = ADVANCED_FACE ( 'NONE', ( #3044 ), #5041, .T. ) ;
#4836 = LINE ( 'NONE', #2710, #19818 ) ;
#4837 = ADVANCED_FACE ( 'NONE', ( #16350 ), #9841, .F. ) ;
#4838 = CARTESIAN_POINT ( 'NONE',  ( 0.000000000000000000, 0.07874015748031495954, 0.000000000000000000 ) ) ;
#4839 = ( CONVERSION_BASED_UNIT ( 'INCH', #1181 ) LENGTH_UNIT ( ) NAMED_UNIT ( #27099 ) ) ;
#4840 = CARTESIAN_POINT ( 'NONE',  ( 0.000000000000000000, 0.000000000000000000, 0.4724409448818898127 ) ) ;
#4841 = CIRCLE ( 'NONE', #7132, 0.3771653543307086909 ) ;
#4842 = DIRECTION ( 'NONE',  ( 0.000000000000000000, 1.000000000000000000, 0.000000000000000000 ) ) ;
#4843 = CARTESIAN_POINT ( 'NONE',  ( -0.6002206662457667541, -0.5625442442678819654, 0.9710808210061889767 ) ) ;
#4844 = AXIS2_PLACEMENT_3D ( 'NONE', #10059, #27596, #27449 ) ;
#4845 = CARTESIAN_POINT ( 'NONE',  ( -0.1570092758121683640, -0.4330450457732857306, 0.1903859678374740794 ) ) ;
#4846 = PRESENTATION_LAYER_ASSIGNMENT (  '', '', ( #3013 ) ) ;
#4847 = PRODUCT_DEFINITION_SHAPE ( 'NONE', 'NONE',  #27893 ) ;
#4848 = DIRECTION ( 'NONE',  ( 0.000000000000000000, 0.000000000000000000, 1.000000000000000000 ) ) ;
#4849 = ORIENTED_EDGE ( 'NONE', *, *, #1377, .T. ) ;
#4850 = CARTESIAN_POINT ( 'NONE',  ( -0.6562077975700097987, -6.248834645669291056E-14, -0.2362204724409449064 ) ) ;
#4851 = VERTEX_POINT ( 'NONE', #7302 ) ;
#4852 = CARTESIAN_POINT ( 'NONE',  ( -0.3349573549949665940, -0.2938049579018697788, -1.934055118110236338 ) ) ;
#4853 = CARTESIAN_POINT ( 'NONE',  ( 0.2420394123212937232, 0.2892587550802425134, 0.07637795275590551769 ) ) ;
#4854 = CARTESIAN_POINT ( 'NONE',  ( -0.5118110236220473341, 0.000000000000000000, -1.550196850393700920 ) ) ;
#4855 = FACE_BOUND ( 'NONE', #27837, .T. ) ;
#4856 = VERTEX_POINT ( 'NONE', #9984 ) ;
#4857 = DIRECTION ( 'NONE',  ( 0.000000000000000000, -1.000000000000000000, 0.000000000000000000 ) ) ;
#4858 = CARTESIAN_POINT ( 'NONE',  ( 0.1153552079389292689, -0.4303653410901767673, -1.934055118110235894 ) ) ;
#4859 = CARTESIAN_POINT ( 'NONE',  ( 0.2296683860596776539, 0.2993674444872277962, -3.100567304031764060 ) ) ;
#4860 = CARTESIAN_POINT ( 'NONE',  ( -1.466875984251968630E-17, 0.000000000000000000, -0.4724409448818898127 ) ) ;
#4861 = DIRECTION ( 'NONE',  ( 0.000000000000000000, 0.000000000000000000, 1.000000000000000000 ) ) ;
#4862 = AXIS2_PLACEMENT_3D ( 'NONE', #3502, #24984, #18472 ) ;
#4863 = EDGE_LOOP ( 'NONE', ( #16587, #345, #25002, #11154 ) ) ;
#4864 = CARTESIAN_POINT ( 'NONE',  ( 0.7165354330708662012, 0.000000000000000000, 0.3425196850393700809 ) ) ;
#4865 = EDGE_CURVE ( 'NONE', #22433, #21273, #24422, .T. ) ;
#4866 = AXIS2_PLACEMENT_3D ( 'NONE', #24813, #7440, #14243 ) ;
#4867 = MECHANICAL_DESIGN_GEOMETRIC_PRESENTATION_REPRESENTATION (  '', ( #9349 ), #13888 ) ;
#4868 = ADVANCED_FACE ( 'NONE', ( #27225 ), #26512, .F. ) ;
#4869 = APPLICATION_PROTOCOL_DEFINITION ( 'draft international standard', 'automotive_design', 1998, #3483 ) ;
#4870 = ORIENTED_EDGE ( 'NONE', *, *, #4591, .T. ) ;
#4871 = VECTOR ( 'NONE', #1562, 39.37007874015748143 ) ;
#4872 = ORIENTED_EDGE ( 'NONE', *, *, #3528, .T. ) ;
#4873 = DIRECTION ( 'NONE',  ( 1.000000000000000000, 7.017815999999999636E-18, 0.000000000000000000 ) ) ;
#4874 = CARTESIAN_POINT ( 'NONE',  ( -0.4472135058506044869, 0.2577577458591217008, 1.766732283464566899 ) ) ;
#4875 = CARTESIAN_POINT ( 'NONE',  ( -0.3855916753051391033, -0.3382184156731863900, 1.747047244094488194 ) ) ;
#4876 = EDGE_CURVE ( 'NONE', #17502, #8729, #24952, .T. ) ;
#4877 = VERTEX_POINT ( 'NONE', #1104 ) ;
#4878 = DIRECTION ( 'NONE',  ( 0.7071067818211385081, 0.7071067805519564153, -8.659560554583433905E-17 ) ) ;
#4879 = EDGE_LOOP ( 'NONE', ( #13228, #15107, #14974, #9118 ) ) ;
#4880 = EDGE_LOOP ( 'NONE', ( #7922, #25227 ) ) ;
#4881 = CARTESIAN_POINT ( 'NONE',  ( 0.3535721684717935132, 0.1200583359873110406, -3.115157480314960647 ) ) ;
#4882 = B_SPLINE_CURVE_WITH_KNOTS ( 'NONE', 3,
 ( #4169, #2450, #21958, #15190, #2041, #8945, #6427, #11205, #4571, #10654 ),
 .UNSPECIFIED., .F., .F.,
 ( 4, 2, 2, 2, 4 ),
 ( 0.000000000000000000, 0.2500000000000000000, 0.5000000000000000000, 0.7500000000000000000, 1.000000000000000000 ),
 .UNSPECIFIED. ) ;
#4883 = EDGE_LOOP ( 'NONE', ( #25142, #5686, #879, #22401 ) ) ;
#4884 = FACE_OUTER_BOUND ( 'NONE', #19252, .T. ) ;
#4885 = DIRECTION ( 'NONE',  ( 0.000000000000000000, 0.000000000000000000, 1.000000000000000000 ) ) ;
#4886 = AXIS2_PLACEMENT_3D ( 'NONE', #20717, #18864, #3757 ) ;
#4887 = CARTESIAN_POINT ( 'NONE',  ( -0.04380447413658832695, 0.3324885138898346360, 1.953740157480315043 ) ) ;
#4888 = EDGE_CURVE ( 'NONE', #16690, #8508, #6581, .T. ) ;
#4889 = ORIENTED_EDGE ( 'NONE', *, *, #27239, .F. ) ;
#4890 = ORIENTED_EDGE ( 'NONE', *, *, #23604, .F. ) ;
#4891 = CIRCLE ( 'NONE', #3444, 0.6881889763779527325 ) ;
#4892 = DIRECTION ( 'NONE',  ( 0.000000000000000000, 0.000000000000000000, 1.000000000000000000 ) ) ;
#4893 = CIRCLE ( 'NONE', #22482, 0.1181102362204720091 ) ;
#4894 = VERTEX_POINT ( 'NONE', #6696 ) ;
#4895 = VERTEX_POINT ( 'NONE', #2174 ) ;
#4896 = EDGE_LOOP ( 'NONE', ( #15308, #27700, #5949, #22955 ) ) ;
#4897 = CIRCLE ( 'NONE', #4010, 0.1308464566929133932 ) ;
#4898 = FACE_OUTER_BOUND ( 'NONE', #11957, .T. ) ;
#4899 = DIRECTION ( 'NONE',  ( -1.000000000000000000, 1.224646799147353454E-16, 0.000000000000000000 ) ) ;
#4900 = CIRCLE ( 'NONE', #8520, 0.01377952755905510404 ) ;
#4901 = CARTESIAN_POINT ( 'NONE',  ( 0.7057179476745132352, 0.7513714478760473714, -0.005393721693867387784 ) ) ;
#4902 = ADVANCED_FACE ( 'NONE', ( #21949 ), #11199, .F. ) ;
#4903 = DIRECTION ( 'NONE',  ( -1.000000000000000000, 0.000000000000000000, 0.000000000000000000 ) ) ;
#4904 = CARTESIAN_POINT ( 'NONE',  ( 0.2669480828848126985, 0.2341512108694336625, 1.953740157480315043 ) ) ;
#4905 = EDGE_CURVE ( 'NONE', #2655, #11023, #16180, .T. ) ;
#4906 = CARTESIAN_POINT ( 'NONE',  ( -0.5610235350335921467, 1.122047331090474165, 0.009609423978176654876 ) ) ;
#4907 = DIRECTION ( 'NONE',  ( 0.000000000000000000, 0.000000000000000000, 1.000000000000000000 ) ) ;
#4908 = AXIS2_PLACEMENT_3D ( 'NONE', #2269, #450, #25873 ) ;
#4909 = FACE_OUTER_BOUND ( 'NONE', #12771, .T. ) ;
#4910 = CIRCLE ( 'NONE', #4023, 0.1673228346456692994 ) ;
#4911 = CARTESIAN_POINT ( 'NONE',  ( -0.3986320731132245165, -0.2308081338369633306, 0.1903859677991110999 ) ) ;
#4912 = CARTESIAN_POINT ( 'NONE',  ( -0.5511811023622047445, 6.750021727583836750E-17, -1.550196850393700920 ) ) ;
#4913 = ORIENTED_EDGE ( 'NONE', *, *, #807, .F. ) ;
#4914 = CARTESIAN_POINT ( 'NONE',  ( 0.4333973147258542991, -0.2509079296564015737, 0.09685039370078740717 ) ) ;
#4915 = STYLED_ITEM ( 'NONE', ( #8655 ), #21329 ) ;
#4916 = CARTESIAN_POINT ( 'NONE',  ( 0.4932821129636645874, 0.08637579872942321990, 0.09685039370078740717 ) ) ;
#4917 = ORIENTED_EDGE ( 'NONE', *, *, #24991, .T. ) ;
#4918 = EDGE_LOOP ( 'NONE', ( #26016, #24345, #19720, #17060, #16164, #5271, #13298, #19391, #25253, #5442, #2817, #17351, #27201, #9989 ) ) ;
#4919 = CARTESIAN_POINT ( 'NONE',  ( 0.1518453844022533417, -0.4909359254662000183, 0.05583672883938764486 ) ) ;
#4920 = ADVANCED_FACE ( 'NONE', ( #20372 ), #16615, .F. ) ;
#4921 = ORIENTED_EDGE ( 'NONE', *, *, #15428, .T. ) ;
#4922 = DIRECTION ( 'NONE',  ( 0.000000000000000000, 0.000000000000000000, -1.000000000000000000 ) ) ;
#4923 = CARTESIAN_POINT ( 'NONE',  ( 0.2705157149885996093, 0.000000000000000000, 0.000000000000000000 ) ) ;
#4924 = ORIENTED_EDGE ( 'NONE', *, *, #16663, .T. ) ;
#4925 = CARTESIAN_POINT ( 'NONE',  ( -0.3362148458988263311, -0.4382482975805425118, 0.9202755905511811330 ) ) ;
#4926 = ORIENTED_EDGE ( 'NONE', *, *, #25976, .F. ) ;
#4927 = CARTESIAN_POINT ( 'NONE',  ( 0.09590060490395689585, -0.2273032555864669124, 2.185478346456692557E-17 ) ) ;
#4928 = VERTEX_POINT ( 'NONE', #7233 ) ;
#4929 = AXIS2_PLACEMENT_3D ( 'NONE', #19766, #433, #15543 ) ;
#4930 = DIRECTION ( 'NONE',  ( 1.000000000000000000, 0.000000000000000000, 0.000000000000000000 ) ) ;
#4931 = AXIS2_PLACEMENT_3D ( 'NONE', #23558, #17182, #23423 ) ;
#4932 = DIRECTION ( 'NONE',  ( 0.000000000000000000, 0.000000000000000000, 1.000000000000000000 ) ) ;
#4933 = DIRECTION ( 'NONE',  ( 0.000000000000000000, -1.000000000000000000, 0.000000000000000000 ) ) ;
#4934 = DIRECTION ( 'NONE',  ( 0.000000000000000000, 0.000000000000000000, -1.000000000000000000 ) ) ;
#4935 = ORIENTED_EDGE ( 'NONE', *, *, #25296, .T. ) ;
#4936 = DIRECTION ( 'NONE',  ( 0.000000000000000000, 1.000000000000000000, 0.000000000000000000 ) ) ;
#4937 = APPLICATION_CONTEXT ( 'automotive_design' ) ;
#4938 = LINE ( 'NONE', #16481, #5532 ) ;
#4939 = FACE_BOUND ( 'NONE', #27144, .T. ) ;
#4940 = ADVANCED_FACE ( 'NONE', ( #13450 ), #5255, .T. ) ;
#4941 = CARTESIAN_POINT ( 'NONE',  ( 0.3520466617656906050, 0.04638120790933070170, 1.953740157480315043 ) ) ;
#4942 = ADVANCED_FACE ( 'NONE', ( #20516 ), #26719, .F. ) ;
#4943 = ORIENTED_EDGE ( 'NONE', *, *, #21983, .T. ) ;
#4944 = DIRECTION ( 'NONE',  ( 1.000000000000000000, 0.000000000000000000, 0.000000000000000000 ) ) ;
#4945 = DIRECTION ( 'NONE',  ( -1.000000000000000000, 0.000000000000000000, 0.000000000000000000 ) ) ;
#4946 = CARTESIAN_POINT ( 'NONE',  ( 0.03736310157557554135, 0.5708661417322835607, 0.9399606299212598381 ) ) ;
#4947 = FACE_OUTER_BOUND ( 'NONE', #10950, .T. ) ;
#4948 = LINE ( 'NONE', #27263, #26804 ) ;
#4949 = ORIENTED_EDGE ( 'NONE', *, *, #11130, .F. ) ;
#4950 = DIRECTION ( 'NONE',  ( 0.000000000000000000, -1.000000000000000000, 0.000000000000000000 ) ) ;
#4951 = AXIS2_PLACEMENT_3D ( 'NONE', #19111, #8108, #17139 ) ;
#4952 = CIRCLE ( 'NONE', #23497, 0.5905511811023621549 ) ;
#4953 = EDGE_LOOP ( 'NONE', ( #14615, #22620 ) ) ;
#4954 = ORIENTED_EDGE ( 'NONE', *, *, #1628, .F. ) ;
#4955 = AXIS2_PLACEMENT_3D ( 'NONE', #7217, #19941, #5237 ) ;
#4956 = CARTESIAN_POINT ( 'NONE',  ( 0.06200787401574775481, 0.000000000000000000, -4.330708661417323135 ) ) ;
#4957 = FACE_OUTER_BOUND ( 'NONE', #2080, .T. ) ;
#4958 = EDGE_LOOP ( 'NONE', ( #27570, #8645, #7902, #4954 ) ) ;
#4959 = CARTESIAN_POINT ( 'NONE',  ( -0.07874015748031511219, 0.1968503937007874127, -3.548228346456693050 ) ) ;
#4960 = ORIENTED_EDGE ( 'NONE', *, *, #17477, .T. ) ;
#4961 = EDGE_CURVE ( 'NONE', #7941, #21315, #21587, .T. ) ;
#4962 = DIRECTION ( 'NONE',  ( -1.000000000000000000, 0.000000000000000000, 0.000000000000000000 ) ) ;
#4963 = CARTESIAN_POINT ( 'NONE',  ( 0.7871730179869745880, 0.2543122156106876197, -0.2818141620071378251 ) ) ;
#4964 = CARTESIAN_POINT ( 'NONE',  ( -0.3264619303874877754, -0.1888818218344748001, 0.1992142436757342316 ) ) ;
#4965 = AXIS2_PLACEMENT_3D ( 'NONE', #19468, #160, #811 ) ;
#4966 = DIRECTION ( 'NONE',  ( 0.000000000000000000, 0.000000000000000000, 1.000000000000000000 ) ) ;
#4967 = DIRECTION ( 'NONE',  ( 0.000000000000000000, -1.000000000000000000, 0.000000000000000000 ) ) ;
#4968 = EDGE_CURVE ( 'NONE', #6094, #25761, #18367, .T. ) ;
#4969 = EDGE_LOOP ( 'NONE', ( #8615, #8882, #20950, #23233 ) ) ;
#4970 = CARTESIAN_POINT ( 'NONE',  ( -0.2211428102655755012, 0.2521176338356572177, 1.973425196850393970 ) ) ;
#4971 = DIRECTION ( 'NONE',  ( -1.224646799147353207E-16, 1.000000000000000000, 0.000000000000000000 ) ) ;
#4972 = CARTESIAN_POINT ( 'NONE',  ( 0.4669911931914963454, -0.1585706980422251222, -1.550196850393700920 ) ) ;
#4973 = CARTESIAN_POINT ( 'NONE',  ( 0.2297883689023126064, 0.3979194638820598984, -1.928289503579157183 ) ) ;
#4974 = AXIS2_PLACEMENT_3D ( 'NONE', #9963, #6026, #18565 ) ;
#4975 = CARTESIAN_POINT ( 'NONE',  ( 0.2442565704126475612, 0.4954197419817565895, 0.9202755905511811330 ) ) ;
#4976 = DIRECTION ( 'NONE',  ( -0.7818314824680298036, 0.6234898018587337054, 0.000000000000000000 ) ) ;
#4977 = DIRECTION ( 'NONE',  ( 0.000000000000000000, 0.000000000000000000, 1.000000000000000000 ) ) ;
#4978 = CARTESIAN_POINT ( 'NONE',  ( 1.197070535079588716, 0.07874015748031491790, -1.315180771300060503 ) ) ;
#4979 = CARTESIAN_POINT ( 'NONE',  ( -0.6112138326843681302, -0.1610742544855759961, 0.2261555117611102339 ) ) ;
#4980 = DIRECTION ( 'NONE',  ( 0.000000000000000000, -1.000000000000000000, 0.000000000000000000 ) ) ;
#4981 = LINE ( 'NONE', #13597, #13625 ) ;
#4982 = CARTESIAN_POINT ( 'NONE',  ( 0.1279527559055118058, 0.000000000000000000, 0.000000000000000000 ) ) ;
#4983 = EDGE_CURVE ( 'NONE', #10848, #1086, #11751, .T. ) ;
#4984 = CARTESIAN_POINT ( 'NONE',  ( 0.1918813796216842782, -0.5271897577243779276, 0.1771653543307086520 ) ) ;
#4985 = CARTESIAN_POINT ( 'NONE',  ( 0.000000000000000000, 0.000000000000000000, 0.2362204724409449064 ) ) ;
#4986 = ORIENTED_EDGE ( 'NONE', *, *, #12754, .F. ) ;
#4987 = CARTESIAN_POINT ( 'NONE',  ( 0.3543307086614173596, 0.000000000000000000, 1.953740157480315043 ) ) ;
#4988 = ORIENTED_EDGE ( 'NONE', *, *, #27217, .F. ) ;
#4989 = DIRECTION ( 'NONE',  ( -1.000000000000000000, -1.224646799147356165E-16, 0.000000000000000000 ) ) ;
#4990 = CARTESIAN_POINT ( 'NONE',  ( 0.1518453844022533417, -0.1971119370939669324, 0.4530813475038464877 ) ) ;
#4991 = DIRECTION ( 'NONE',  ( 0.000000000000000000, -1.000000000000000000, 0.000000000000000000 ) ) ;
#4992 = ORIENTED_EDGE ( 'NONE', *, *, #18076, .F. ) ;
#4993 = CARTESIAN_POINT ( 'NONE',  ( 0.000000000000000000, 0.000000000000000000, 0.3425196850393700809 ) ) ;
#4994 = CYLINDRICAL_SURFACE ( 'NONE', #12683, 0.1181102362204718703 ) ;
#4995 = EDGE_CURVE ( 'NONE', #550, #15456, #17942, .T. ) ;
#4996 = CARTESIAN_POINT ( 'NONE',  ( 0.000000000000000000, 0.000000000000000000, -4.015748031496062964 ) ) ;
#4997 = CARTESIAN_POINT ( 'NONE',  ( -0.05118110236220472370, 0.000000000000000000, 0.000000000000000000 ) ) ;
#4998 = CARTESIAN_POINT ( 'NONE',  ( 0.1213180142433946118, -0.3572819248074403653, -3.100567304031765392 ) ) ;
#4999 = ADVANCED_FACE ( 'NONE', ( #11896, #18075 ), #24327, .T. ) ;
#5000 = CARTESIAN_POINT ( 'NONE',  ( 3.644242538420618632E-18, 0.5007874015748032814, 0.09684793308443545579 ) ) ;
#5001 = CARTESIAN_POINT ( 'NONE',  ( 0.000000000000000000, 0.000000000000000000, 0.2362204724409449064 ) ) ;
#5002 = ORIENTED_EDGE ( 'NONE', *, *, #16148, .F. ) ;
#5003 = CARTESIAN_POINT ( 'NONE',  ( 0.5925575908939920700, 0.000000000000000000, 0.000000000000000000 ) ) ;
#5004 = AXIS2_PLACEMENT_3D ( 'NONE', #6179, #23951, #19289 ) ;
#5005 = APPLICATION_PROTOCOL_DEFINITION ( 'draft international standard', 'automotive_design', 1998, #14882 ) ;
#5006 = CIRCLE ( 'NONE', #5947, 1.288838582677165556 ) ;
#5007 = VERTEX_POINT ( 'NONE', #13730 ) ;
#5008 = TOROIDAL_SURFACE ( 'NONE', #27072, 0.8031496062992127261, 0.02362204724409448786 ) ;
#5009 = SPHERICAL_SURFACE ( 'NONE', #24579, 0.1003956692913385851 ) ;
#5010 = DIRECTION ( 'NONE',  ( -1.000000000000000000, 0.000000000000000000, 0.000000000000000000 ) ) ;
#5011 = CARTESIAN_POINT ( 'NONE',  ( -0.3121994997597934973, 0.4069448477556333321, 1.747047244094488194 ) ) ;
#5012 = LENGTH_MEASURE_WITH_UNIT ( LENGTH_MEASURE( 0.02539999999999999897 ), #19597 ) ;
#5013 = ORIENTED_EDGE ( 'NONE', *, *, #24359, .T. ) ;
#5014 = CARTESIAN_POINT ( 'NONE',  ( -0.3765118517642104257, 0.000000000000000000, -3.100567304031763172 ) ) ;
#5015 = DIRECTION ( 'NONE',  ( 0.000000000000000000, -1.000000000000000000, 0.000000000000000000 ) ) ;
#5016 = ORIENTED_EDGE ( 'NONE', *, *, #7452, .F. ) ;
#5017 = DIRECTION ( 'NONE',  ( -1.000000000000000000, 0.000000000000000000, 0.000000000000000000 ) ) ;
#5018 = CARTESIAN_POINT ( 'NONE',  ( -2.183966630091013010E-17, 0.6212598425196852459, 0.09684793308443542803 ) ) ;
#5019 = ORIENTED_EDGE ( 'NONE', *, *, #23730, .F. ) ;
#5020 = CARTESIAN_POINT ( 'NONE',  ( 0.1078280746903977072, 0.3175540113612247972, 1.953740157480315043 ) ) ;
#5021 = ORIENTED_EDGE ( 'NONE', *, *, #17755, .T. ) ;
#5022 = ORIENTED_EDGE ( 'NONE', *, *, #1850, .F. ) ;
#5023 = VERTEX_POINT ( 'NONE', #2839 ) ;
#5024 = EDGE_CURVE ( 'NONE', #23096, #19036, #26141, .T. ) ;
#5025 = CIRCLE ( 'NONE', #19920, 1.377952755905512472 ) ;
#5026 = CARTESIAN_POINT ( 'NONE',  ( 0.5511811023622048555, 6.829619984160658046E-17, 0.9399606299212598381 ) ) ;
#5027 = EDGE_LOOP ( 'NONE', ( #9275, #3316, #17408, #8169 ) ) ;
#5028 = CARTESIAN_POINT ( 'NONE',  ( -0.05819755867303792046, 0.4417361510194100505, -1.934055118110236338 ) ) ;
#5029 = EDGE_LOOP ( 'NONE', ( #12681, #25468, #3492, #692 ) ) ;
#5030 = ORIENTED_EDGE ( 'NONE', *, *, #12576, .T. ) ;
#5031 = CARTESIAN_POINT ( 'NONE',  ( 0.000000000000000000, -0.2273032555864669124, 3.963736220472441631E-17 ) ) ;
#5032 = DIRECTION ( 'NONE',  ( 0.1736481776669309696, 0.9848077530122079093, 0.000000000000000000 ) ) ;
#5033 = EDGE_CURVE ( 'NONE', #20898, #22611, #3998, .T. ) ;
#5034 = AXIS2_PLACEMENT_3D ( 'NONE', #5818, #27283, #27147 ) ;
#5035 = AXIS2_PLACEMENT_3D ( 'NONE', #23800, #15468, #4447 ) ;
#5036 = CARTESIAN_POINT ( 'NONE',  ( -0.3574975638436101444, 0.000000000000000000, -3.115157480314960647 ) ) ;
#5037 = DIRECTION ( 'NONE',  ( 1.224646799147353207E-16, 1.000000000000000000, -0.000000000000000000 ) ) ;
#5038 = FACE_OUTER_BOUND ( 'NONE', #20604, .T. ) ;
#5039 = ORIENTED_EDGE ( 'NONE', *, *, #22013, .F. ) ;
#5040 = DIRECTION ( 'NONE',  ( -0.000000000000000000, -0.000000000000000000, -1.000000000000000000 ) ) ;
#5041 = CYLINDRICAL_SURFACE ( 'NONE', #409, 0.2395669291338582696 ) ;
#5042 = CARTESIAN_POINT ( 'NONE',  ( 0.7874015748031496509, 1.344047637795275569E-32, 0.2362204724409449064 ) ) ;
#5043 = CIRCLE ( 'NONE', #19028, 0.6212598425196850238 ) ;
#5044 = DIRECTION ( 'NONE',  ( 0.000000000000000000, 0.000000000000000000, -1.000000000000000000 ) ) ;
#5045 = CARTESIAN_POINT ( 'NONE',  ( -0.05945372446461825305, -0.05659567841061365762, -0.4680802598521939806 ) ) ;
#5046 = CARTESIAN_POINT ( 'NONE',  ( 0.1516263115863346334, 0.4909405214979283838, -0.05579628926458630317 ) ) ;
#5047 = CARTESIAN_POINT ( 'NONE',  ( 0.3242071728275122688, 0.4225965726692672564, 1.747047244094488194 ) ) ;
#5048 = VECTOR ( 'NONE', #17907, 39.37007874015748143 ) ;
#5049 = B_SPLINE_CURVE_WITH_KNOTS ( 'NONE', 3,
 ( #6035, #14526, #9835, #20998, #10245, #14671, #3321, #3608, #12097, #5467, #23129, #18433, #23275, #12238, #21138, #3904, #14377, #1643 ),
 .UNSPECIFIED., .F., .F.,
 ( 4, 2, 2, 2, 2, 2, 2, 2, 4 ),
 ( 0.5000000000000000000, 0.5625000000000000000, 0.6250000000000000000, 0.6875000000000000000, 0.7500000000000000000, 0.8125000000000000000, 0.8750000000000001110, 0.9375000000000001110, 1.000000000000000000 ),
 .UNSPECIFIED. ) ;
#5050 = CARTESIAN_POINT ( 'NONE',  ( -0.2952755905264887182, 3.616083068046089993E-17, -2.322834645648386154 ) ) ;
#5051 = ORIENTED_EDGE ( 'NONE', *, *, #20893, .F. ) ;
#5052 = CARTESIAN_POINT ( 'NONE',  ( 0.6397637795275591399, 0.000000000000000000, 0.000000000000000000 ) ) ;
#5053 = ORIENTED_EDGE ( 'NONE', *, *, #16911, .T. ) ;
#5054 = FACE_OUTER_BOUND ( 'NONE', #11043, .T. ) ;
#5055 = ORIENTED_EDGE ( 'NONE', *, *, #15114, .F. ) ;
#5056 = EDGE_CURVE ( 'NONE', #14228, #10058, #13664, .T. ) ;
#5057 = CARTESIAN_POINT ( 'NONE',  ( 0.3912931228432083297, 0.3001918266902350307, -1.569881889763779625 ) ) ;
#5058 = CARTESIAN_POINT ( 'NONE',  ( 0.7214243740402349614, -0.1654689342656808781, 0.2562996996016383422 ) ) ;
#5059 = ORIENTED_EDGE ( 'NONE', *, *, #16111, .T. ) ;
#5060 = CARTESIAN_POINT ( 'NONE',  ( -0.07214854559199535000, -0.5476281405333250918, 0.9399606299212598381 ) ) ;
#5061 = ORIENTED_EDGE ( 'NONE', *, *, #2374, .F. ) ;
#5062 = EDGE_CURVE ( 'NONE', #24230, #3515, #24729, .T. ) ;
#5063 = CIRCLE ( 'NONE', #3252, 0.5322834645669292097 ) ;
#5064 = DIRECTION ( 'NONE',  ( 0.000000000000000000, 0.000000000000000000, 1.000000000000000000 ) ) ;
#5065 = PLANE ( 'NONE',  #10827 ) ;
#5066 = DIRECTION ( 'NONE',  ( 1.000000000000000000, 0.000000000000000000, 0.000000000000000000 ) ) ;
#5067 = CARTESIAN_POINT ( 'NONE',  ( 0.000000000000000000, 0.000000000000000000, 0.3425196850393700809 ) ) ;
#5068 = CARTESIAN_POINT ( 'NONE',  ( -0.3992017438595021339, -0.2298214351608249550, 0.1903859677995012600 ) ) ;
#5069 = TOROIDAL_SURFACE ( 'NONE', #20425, 0.4232283464566928832, 0.07677165354330708902 ) ;
#5070 = CARTESIAN_POINT ( 'NONE',  ( -0.2362204724409449064, 1.131889763779527547, 0.000000000000000000 ) ) ;
#5071 = EDGE_CURVE ( 'NONE', #26781, #27801, #26866, .T. ) ;
#5072 = VERTEX_POINT ( 'NONE', #7807 ) ;
#5073 = FACE_OUTER_BOUND ( 'NONE', #17401, .T. ) ;
#5074 = CARTESIAN_POINT ( 'NONE',  ( 0.6299212598425196763, 0.000000000000000000, -0.3740157480314960647 ) ) ;
#5075 = CARTESIAN_POINT ( 'NONE',  ( -1.355511558298621910, 1.564461769117756029, 2.027559055118110187 ) ) ;
#5076 = CARTESIAN_POINT ( 'NONE',  ( -0.03001016326913665336, -0.4585215200179055817, -1.928289503579156516 ) ) ;
#5077 = DIRECTION ( 'NONE',  ( 0.000000000000000000, 1.000000000000000000, 0.000000000000000000 ) ) ;
#5078 = CARTESIAN_POINT ( 'NONE',  ( -0.07874015748031511219, 0.1968503937007874127, -3.548228346456693050 ) ) ;
#5079 = PRODUCT_DEFINITION_SHAPE ( 'NONE', 'NONE',  #6545 ) ;
#5080 = DIRECTION ( 'NONE',  ( 0.000000000000000000, 0.000000000000000000, -1.000000000000000000 ) ) ;
#5081 = CONICAL_SURFACE ( 'NONE', #25851, 0.2952755905264887182, 0.2617993876495733341 ) ;
#5082 = AXIS2_PLACEMENT_3D ( 'NONE', #5721, #25337, #1469 ) ;
#5083 = ORIENTED_EDGE ( 'NONE', *, *, #19523, .F. ) ;
#5084 = VERTEX_POINT ( 'NONE', #23364 ) ;
#5085 = AXIS2_PLACEMENT_3D ( 'NONE', #24163, #22043, #26013 ) ;
#5086 = CARTESIAN_POINT ( 'NONE',  ( 0.000000000000000000, 0.000000000000000000, 39.92337183164450920 ) ) ;
#5087 = ( REPRESENTATION_RELATIONSHIP ('NONE','NONE', #12434, #16232 ) REPRESENTATION_RELATIONSHIP_WITH_TRANSFORMATION ( #25556 )SHAPE_REPRESENTATION_RELATIONSHIP( ) ) ;
#5088 = CARTESIAN_POINT ( 'NONE',  ( 0.000000000000000000, 0.000000000000000000, -0.2480314960629921295 ) ) ;
#5089 = ORIENTED_EDGE ( 'NONE', *, *, #18442, .T. ) ;
#5090 = EDGE_CURVE ( 'NONE', #12575, #5387, #20154, .T. ) ;
#5091 = DIRECTION ( 'NONE',  ( 0.000000000000000000, 0.000000000000000000, 1.000000000000000000 ) ) ;
#5092 = ORIENTED_EDGE ( 'NONE', *, *, #10873, .T. ) ;
#5093 = EDGE_CURVE ( 'NONE', #13737, #15651, #22932, .T. ) ;
#5094 = CARTESIAN_POINT ( 'NONE',  ( 0.6175000359513720394, 0.5724198758948899624, -0.4671145582681361375 ) ) ;
#5095 = AXIS2_PLACEMENT_3D ( 'NONE', #4473, #9480, #20093 ) ;
#5096 = AXIS2_PLACEMENT_3D ( 'NONE', #26432, #24876, #22626 ) ;
#5097 = CARTESIAN_POINT ( 'NONE',  ( 0.5925575908939920700, 0.000000000000000000, 0.000000000000000000 ) ) ;
#5098 = ORIENTED_EDGE ( 'NONE', *, *, #16663, .F. ) ;
#5099 = CARTESIAN_POINT ( 'NONE',  ( 0.09522041251245175197, 0.3002250111098912488, -3.573961723184375661 ) ) ;
#5100 = CARTESIAN_POINT ( 'NONE',  ( 0.3121994997578272368, 0.4069448477569235778, -1.550196850393700920 ) ) ;
#5101 = CARTESIAN_POINT ( 'NONE',  ( -0.2297883689023087483, 0.3979194638820583441, -1.928289503579160513 ) ) ;
#5102 = TOROIDAL_SURFACE ( 'NONE', #9177, 0.4232283464566928832, 0.07677165354330708902 ) ;
#5103 = DIRECTION ( 'NONE',  ( 1.000000000000000000, 0.000000000000000000, 0.000000000000000000 ) ) ;
#5104 = CARTESIAN_POINT ( 'NONE',  ( 0.3362148458988418187, -0.4382482975805321312, 0.9202755905511811330 ) ) ;
#5105 = CARTESIAN_POINT ( 'NONE',  ( 0.6119360453657027854, 0.1072290460172409393, 0.2574803149606298969 ) ) ;
#5106 = VECTOR ( 'NONE', #7203, 39.37007874015748854 ) ;
#5107 = CARTESIAN_POINT ( 'NONE',  ( 0.000000000000000000, 0.000000000000000000, 0.1322834645669291320 ) ) ;
#5108 = CARTESIAN_POINT ( 'NONE',  ( -0.5614173959491228771, 0.4467232815856471695, 0.3122824329321748915 ) ) ;
#5109 = CONICAL_SURFACE ( 'NONE', #26758, 0.8214970631411201429, 0.2617993875000020898 ) ;
#5110 = ADVANCED_FACE ( 'NONE', ( #23069 ), #9372, .F. ) ;
#5111 = CARTESIAN_POINT ( 'NONE',  ( 2.664928230027803213, 0.9448818897637796255, -0.1082677165354330867 ) ) ;
#5112 = DIRECTION ( 'NONE',  ( 0.8660254037844385966, -0.5000000000000000000, 0.000000000000000000 ) ) ;
#5113 = CARTESIAN_POINT ( 'NONE',  ( 0.4898768902087983768, 0.000000000000000000, 0.2362204724409449064 ) ) ;
#5114 = CARTESIAN_POINT ( 'NONE',  ( 0.2239856983831502169, -0.4635973202131455917, 0.1473214333510785012 ) ) ;
#5115 = LINE ( 'NONE', #18377, #5515 ) ;
#5116 = DIRECTION ( 'NONE',  ( -0.000000000000000000, 1.000000000000000000, -0.000000000000000000 ) ) ;
#5117 = AXIS2_PLACEMENT_3D ( 'NONE', #22324, #19928, #7207 ) ;
#5118 = EDGE_CURVE ( 'NONE', #11020, #16931, #18720, .T. ) ;
#5119 = CARTESIAN_POINT ( 'NONE',  ( 0.1610509776512594748, -0.4407912692718567449, 0.1992125984251968684 ) ) ;
#5120 = ORIENTED_EDGE ( 'NONE', *, *, #18963, .T. ) ;
#5121 = CARTESIAN_POINT ( 'NONE',  ( -1.466875984251968630E-17, 0.000000000000000000, -0.02362204724409448786 ) ) ;
#5122 = ORIENTED_EDGE ( 'NONE', *, *, #5965, .F. ) ;
#5123 = DIRECTION ( 'NONE',  ( -1.000000000000000000, 0.000000000000000000, 0.000000000000000000 ) ) ;
#5124 = ORIENTED_EDGE ( 'NONE', *, *, #22846, .T. ) ;
#5125 = AXIS2_PLACEMENT_3D ( 'NONE', #13732, #11340, #15599 ) ;
#5126 = CARTESIAN_POINT ( 'NONE',  ( 0.2991932138496286586, -0.3411003281197161341, -1.934055118110236338 ) ) ;
#5127 = CARTESIAN_POINT ( 'NONE',  ( 0.0006479495459697544183, 0.5014297259257108896, 0.3080453759639392719 ) ) ;
#5128 = DIRECTION ( 'NONE',  ( 0.000000000000000000, 0.000000000000000000, -1.000000000000000000 ) ) ;
#5129 = CARTESIAN_POINT ( 'NONE',  ( 0.09524629980714841015, 0.3002167689318728239, -3.247000705324971648 ) ) ;
#5130 = VECTOR ( 'NONE', #4991, 39.37007874015748143 ) ;
#5131 = CARTESIAN_POINT ( 'NONE',  ( 0.1504231045792249755, 0.2090266774008008310, 0.4379142800569870153 ) ) ;
#5132 = CARTESIAN_POINT ( 'NONE',  ( 0.000000000000000000, 0.000000000000000000, -0.2480314960629921295 ) ) ;
#5133 = CARTESIAN_POINT ( 'NONE',  ( 0.5869493968219645641, 0.000000000000000000, 0.000000000000000000 ) ) ;
#5134 = CARTESIAN_POINT ( 'NONE',  ( -0.3534612032199798692, -0.2712680014832878905, -1.934055118110236560 ) ) ;
#5135 = CARTESIAN_POINT ( 'NONE',  ( -0.1213180142433854664, 0.3572819248074437515, -3.100567304031767168 ) ) ;
#5136 = CARTESIAN_POINT ( 'NONE',  ( 0.5925575908939920700, 0.2268709785195984208, -0.3929520615588126264 ) ) ;
#5137 = AXIS2_PLACEMENT_3D ( 'NONE', #27832, #8468, #4238 ) ;
#5138 = VERTEX_POINT ( 'NONE', #6122 ) ;
#5139 = CARTESIAN_POINT ( 'NONE',  ( -7.608238775805210269E-17, -0.6212598425196850238, 0.09685039370078740717 ) ) ;
#5140 = CARTESIAN_POINT ( 'NONE',  ( -0.2796934465393772773, -0.3645739570812616681, -1.928289503579163178 ) ) ;
#5141 = DIRECTION ( 'NONE',  ( 1.000000000000000000, 0.000000000000000000, 0.000000000000000000 ) ) ;
#5142 = EDGE_CURVE ( 'NONE', #26728, #9665, #11645, .T. ) ;
#5143 = CONICAL_SURFACE ( 'NONE', #20951, 0.4724409448465559103, 0.7853981642948979491 ) ;
#5144 = ORIENTED_EDGE ( 'NONE', *, *, #2432, .T. ) ;
#5145 = CIRCLE ( 'NONE', #3817, 0.5379714048901780288 ) ;
#5146 = B_SPLINE_CURVE_WITH_KNOTS ( 'NONE', 3,
 ( #1782, #27650, #2602, #17717, #22108, #505, #11228, #13622, #26339, #17848 ),
 .UNSPECIFIED., .F., .F.,
 ( 4, 2, 2, 2, 4 ),
 ( 0.000000000000000000, 0.2500000000000000000, 0.5000000000000000000, 0.7500000000000000000, 1.000000000000000000 ),
 .UNSPECIFIED. ) ;
#5147 = CARTESIAN_POINT ( 'NONE',  ( 0.09842519685039366473, 0.1968503937007873850, -3.456364829396326943 ) ) ;
#5148 = CARTESIAN_POINT ( 'NONE',  ( 0.5869493968219645641, -0.4267795243146149664, 5.226543307086613929E-17 ) ) ;
#5149 = CARTESIAN_POINT ( 'NONE',  ( -0.4600326175560703335, -0.2268096725222389642, 1.747047244094488194 ) ) ;
#5150 = EDGE_CURVE ( 'NONE', #764, #2591, #20734, .T. ) ;
#5151 = ORIENTED_EDGE ( 'NONE', *, *, #16475, .T. ) ;
#5152 = DIRECTION ( 'NONE',  ( 0.7818314824680300257, 0.6234898018587330393, -0.000000000000000000 ) ) ;
#5153 = CARTESIAN_POINT ( 'NONE',  ( -0.1651192144506347381, 0.3349073414798414139, -3.115157480314960647 ) ) ;
#5154 = ADVANCED_FACE ( 'NONE', ( #1439 ), #7948, .T. ) ;
#5155 = ORIENTED_EDGE ( 'NONE', *, *, #19745, .T. ) ;
#5156 = CARTESIAN_POINT ( 'NONE',  ( -0.6209926255554318875, 1.097802432539390916, -0.08994119036278866441 ) ) ;
#5157 = CARTESIAN_POINT ( 'NONE',  ( -0.3180687940157840843, 0.000000000000000000, -0.04133858267716535029 ) ) ;
#5158 = AXIS2_PLACEMENT_3D ( 'NONE', #4510, #15126, #12978 ) ;
#5159 = ORIENTED_EDGE ( 'NONE', *, *, #26948, .F. ) ;
#5160 = ORIENTED_EDGE ( 'NONE', *, *, #25897, .T. ) ;
#5161 = CARTESIAN_POINT ( 'NONE',  ( -0.3969055948396000288, -0.6093040995678481453, -0.5087267836413271738 ) ) ;
#5162 = CARTESIAN_POINT ( 'NONE',  ( -0.5511811023622047445, -1.131889763744194921, 0.000000000000000000 ) ) ;
#5163 = ORIENTED_EDGE ( 'NONE', *, *, #23351, .T. ) ;
#5164 = CARTESIAN_POINT ( 'NONE',  ( 0.3349573549949907414, 0.2938049579018708890, -1.934055118110236338 ) ) ;
#5165 = EDGE_LOOP ( 'NONE', ( #21509, #19526, #11232, #27712, #14926 ) ) ;
#5166 = ORIENTED_EDGE ( 'NONE', *, *, #2485, .F. ) ;
#5167 = CARTESIAN_POINT ( 'NONE',  ( -0.3131893444210941957, 0.3723335979309581600, 0.1075369453644233753 ) ) ;
#5168 = FACE_BOUND ( 'NONE', #9635, .T. ) ;
#5169 = CIRCLE ( 'NONE', #26382, 0.3346456692913385988 ) ;
#5170 = CARTESIAN_POINT ( 'NONE',  ( -0.03794311743615354227, 0.7585235100853641166, -0.4108618826768283827 ) ) ;
#5171 = AXIS2_PLACEMENT_3D ( 'NONE', #27510, #18866, #6184 ) ;
#5172 = DIRECTION ( 'NONE',  ( 0.000000000000000000, 0.000000000000000000, -1.000000000000000000 ) ) ;
#5173 = DIRECTION ( 'NONE',  ( 0.000000000000000000, -1.000000000000000000, 0.000000000000000000 ) ) ;
#5174 = EDGE_CURVE ( 'NONE', #27602, #1942, #15289, .T. ) ;
#5175 = DIRECTION ( 'NONE',  ( -1.000000000000000000, 0.000000000000000000, 0.000000000000000000 ) ) ;
#5176 = CARTESIAN_POINT ( 'NONE',  ( 0.6514872030421683391, 0.1141809932449793924, 0.1616495878895669036 ) ) ;
#5177 = SURFACE_STYLE_FILL_AREA ( #25489 ) ;
#5178 = CARTESIAN_POINT ( 'NONE',  ( -0.2341512108694376038, 0.2669480828848188603, 1.953740157480315043 ) ) ;
#5179 = AXIS2_PLACEMENT_3D ( 'NONE', #24097, #13628, #21710 ) ;
#5180 = DIRECTION ( 'NONE',  ( 0.000000000000000000, 1.000000000000000000, 0.000000000000000000 ) ) ;
#5181 = EDGE_CURVE ( 'NONE', #22055, #1806, #23436, .T. ) ;
#5182 = DIRECTION ( 'NONE',  ( 0.000000000000000000, 0.000000000000000000, 1.000000000000000000 ) ) ;
#5183 = CARTESIAN_POINT ( 'NONE',  ( -0.009795313329541911057, -0.08526597544697904485, -0.4724409448818898127 ) ) ;
#5184 = FACE_OUTER_BOUND ( 'NONE', #16091, .T. ) ;
#5185 = CARTESIAN_POINT ( 'NONE',  ( -0.2663596103035606455, 0.4612490782034870396, 1.747047244094488194 ) ) ;
#5186 = EDGE_CURVE ( 'NONE', #19404, #24230, #14719, .T. ) ;
#5187 = CARTESIAN_POINT ( 'NONE',  ( 0.2564944395515608710, 0.4441657790107836346, 1.766732283464566899 ) ) ;
#5188 = ORIENTED_EDGE ( 'NONE', *, *, #10508, .T. ) ;
#5189 = AXIS2_PLACEMENT_3D ( 'NONE', #220, #2156, #6541 ) ;
#5190 = PLANE ( 'NONE',  #11970 ) ;
#5191 = ORIENTED_EDGE ( 'NONE', *, *, #1249, .T. ) ;
#5192 = EDGE_CURVE ( 'NONE', #27168, #3201, #14400, .T. ) ;
#5193 = AXIS2_PLACEMENT_3D ( 'NONE', #13555, #2541, #9301 ) ;
#5194 = DIRECTION ( 'NONE',  ( -0.5000000010362850578, 0.8660254031861391866, 0.000000000000000000 ) ) ;
#5195 = ORIENTED_EDGE ( 'NONE', *, *, #27799, .F. ) ;
#5196 = DIRECTION ( 'NONE',  ( 0.000000000000000000, -1.000000000000000000, 0.000000000000000000 ) ) ;
#5197 = EDGE_CURVE ( 'NONE', #13825, #8723, #4891, .T. ) ;
#5198 = ORIENTED_EDGE ( 'NONE', *, *, #4258, .F. ) ;
#5199 = CARTESIAN_POINT ( 'NONE',  ( 0.3252100150720242944, 0.3707612262533179215, -1.569881889763779625 ) ) ;
#5200 = CARTESIAN_POINT ( 'NONE',  ( -0.3411065095061437957, 0.06065137456822555090, 0.1377952755905512139 ) ) ;
#5201 = ORIENTED_EDGE ( 'NONE', *, *, #17489, .T. ) ;
#5202 = CARTESIAN_POINT ( 'NONE',  ( -0.4783323773986942751, -0.2762247810518927427, 0.9399606299212598381 ) ) ;
#5203 = ORIENTED_EDGE ( 'NONE', *, *, #20343, .T. ) ;
#5204 = ORIENTED_EDGE ( 'NONE', *, *, #17454, .F. ) ;
#5205 = VECTOR ( 'NONE', #11552, 39.37007874015748143 ) ;
#5206 = CARTESIAN_POINT ( 'NONE',  ( 0.4165721057576322606, 0.3313508221749649763, 0.3401574803149606252 ) ) ;
#5207 = EDGE_CURVE ( 'NONE', #24495, #7391, #25132, .T. ) ;
#5208 = LINE ( 'NONE', #13831, #24858 ) ;
#5209 = FACE_BOUND ( 'NONE', #24077, .T. ) ;
#5210 = DIRECTION ( 'NONE',  ( 1.000000000000000000, 0.000000000000000000, 0.000000000000000000 ) ) ;
#5211 = DIRECTION ( 'NONE',  ( 0.000000000000000000, 1.224646799147355919E-16, 1.000000000000000000 ) ) ;
#5212 = CARTESIAN_POINT ( 'NONE',  ( 0.2395669291338582696, 2.933848729453403498E-17, -0.4566929133858267376 ) ) ;
#5213 = CARTESIAN_POINT ( 'NONE',  ( 0.05945372446461825305, 0.05659567841061365762, -0.4680802598521939806 ) ) ;
#5214 = CARTESIAN_POINT ( 'NONE',  ( -0.1285103288269285327, -0.3545966721392122545, 0.07637795275590551769 ) ) ;
#5215 = CIRCLE ( 'NONE', #25540, 0.6212598425196850238 ) ;
#5216 = CARTESIAN_POINT ( 'NONE',  ( 0.2904160862623607620, -0.1677079028045494191, 1.953740157480315043 ) ) ;
#5217 = ORIENTED_EDGE ( 'NONE', *, *, #25937, .T. ) ;
#5218 = CARTESIAN_POINT ( 'NONE',  ( 0.000000000000000000, 0.000000000000000000, -4.330708661417323135 ) ) ;
#5219 = DIRECTION ( 'NONE',  ( 1.000000000000000000, 0.000000000000000000, 0.000000000000000000 ) ) ;
#5220 = ADVANCED_FACE ( 'NONE', ( #3224, #26412 ), #22182, .T. ) ;
#5221 = AXIS2_PLACEMENT_3D ( 'NONE', #25419, #6219, #6393 ) ;
#5222 = CARTESIAN_POINT ( 'NONE',  ( -0.6226845887534185886, -0.1205360030604272631, 0.2306066678346231080 ) ) ;
#5223 = CYLINDRICAL_SURFACE ( 'NONE', #6747, 0.3937007873768824662 ) ;
#5224 = CARTESIAN_POINT ( 'NONE',  ( 0.2169784220074747749, -0.4520537072447231020, 0.3080453759200848518 ) ) ;
#5225 = FACE_OUTER_BOUND ( 'NONE', #19319, .T. ) ;
#5226 = DIRECTION ( 'NONE',  ( 1.224646799147353207E-16, 1.000000000000000000, -0.000000000000000000 ) ) ;
#5227 = EDGE_CURVE ( 'NONE', #21275, #20990, #3873, .T. ) ;
#5228 = CARTESIAN_POINT ( 'NONE',  ( -0.2997912780622379314, -0.1736589463928940036, 0.1276989850587680886 ) ) ;
#5229 = CARTESIAN_POINT ( 'NONE',  ( 0.000000000000000000, 0.000000000000000000, 0.000000000000000000 ) ) ;
#5230 = EDGE_CURVE ( 'NONE', #11142, #2922, #10315, .T. ) ;
#5231 = EDGE_LOOP ( 'NONE', ( #10752, #21180, #5159, #27091 ) ) ;
#5232 = FACE_OUTER_BOUND ( 'NONE', #16959, .T. ) ;
#5233 = AXIS2_PLACEMENT_3D ( 'NONE', #25993, #21482, #8208 ) ;
#5234 = DIRECTION ( 'NONE',  ( -1.000000000000000000, 0.000000000000000000, 0.000000000000000000 ) ) ;
#5235 = ORIENTED_EDGE ( 'NONE', *, *, #8944, .T. ) ;
#5236 = LINE ( 'NONE', #16266, #25041 ) ;
#5237 = DIRECTION ( 'NONE',  ( 0.000000000000000000, -1.000000000000000000, 0.000000000000000000 ) ) ;
#5238 = ORIENTED_EDGE ( 'NONE', *, *, #16122, .F. ) ;
#5239 = ADVANCED_FACE ( 'NONE', ( #4947 ), #24748, .F. ) ;
#5240 = VECTOR ( 'NONE', #27035, 39.37007874015748854 ) ;
#5241 = FILL_AREA_STYLE ('',( #3241 ) ) ;
#5242 = CARTESIAN_POINT ( 'NONE',  ( 0.7874015748031325534, 0.3451340551350263741, 0.02485503895194105320 ) ) ;
#5243 = CARTESIAN_POINT ( 'NONE',  ( 0.1896185148830507872, 0.3289909311256233870, -3.100567304031763172 ) ) ;
#5244 = CARTESIAN_POINT ( 'NONE',  ( 0.2992781133268291316, -0.6197069291944922176, 0.1322834645669291320 ) ) ;
#5245 = ORIENTED_EDGE ( 'NONE', *, *, #8116, .T. ) ;
#5246 = ORIENTED_EDGE ( 'NONE', *, *, #416, .F. ) ;
#5247 = ORIENTED_EDGE ( 'NONE', *, *, #19961, .T. ) ;
#5248 = CARTESIAN_POINT ( 'NONE',  ( -0.1677079028045370956, -0.2904160862623674233, 1.973425196850393970 ) ) ;
#5249 = DIRECTION ( 'NONE',  ( -1.000000000000000000, 0.000000000000000000, 0.000000000000000000 ) ) ;
#5250 = CARTESIAN_POINT ( 'NONE',  ( -0.4069448477569480582, 0.3121994997578198539, -1.550196850393700920 ) ) ;
#5251 = DIRECTION ( 'NONE',  ( -1.000000000000000000, 0.000000000000000000, 0.000000000000000000 ) ) ;
#5252 = EDGE_CURVE ( 'NONE', #8729, #15321, #27474, .T. ) ;
#5253 = AXIS2_PLACEMENT_3D ( 'NONE', #2950, #5655, #14279 ) ;
#5254 = CARTESIAN_POINT ( 'NONE',  ( 0.3362148458988273303, 0.4382482975805419012, 0.9202755905511811330 ) ) ;
#5255 = CYLINDRICAL_SURFACE ( 'NONE', #14837, 0.5905511811023621549 ) ;
#5256 = AXIS2_PLACEMENT_3D ( 'NONE', #11090, #632, #24081 ) ;
#5257 = CARTESIAN_POINT ( 'NONE',  ( 1.197070535079588716, 0.4724409448818898127, -1.197070535079588716 ) ) ;
#5258 = CARTESIAN_POINT ( 'NONE',  ( -0.2303471512294322787, -0.4798602677570401598, 0.3401574803149606252 ) ) ;
#5259 = EDGE_CURVE ( 'NONE', #19876, #1085, #8286, .T. ) ;
#5260 = AXIS2_PLACEMENT_3D ( 'NONE', #17991, #21328, #18151 ) ;
#5261 = ADVANCED_FACE ( 'NONE', ( #8063 ), #20627, .T. ) ;
#5262 = CARTESIAN_POINT ( 'NONE',  ( 2.531258147843938596E-16, 0.3937007873309092409, 2.066929133858267598 ) ) ;
#5263 = LINE ( 'NONE', #13881, #2046 ) ;
#5264 = CARTESIAN_POINT ( 'NONE',  ( 0.000000000000000000, 0.000000000000000000, 0.1322834645669291320 ) ) ;
#5265 = CARTESIAN_POINT ( 'NONE',  ( 0.3998447049182496382, 0.4754871227240771714, 0.09685039370078740717 ) ) ;
#5266 = VERTEX_POINT ( 'NONE', #12140 ) ;
#5267 = VERTEX_POINT ( 'NONE', #9743 ) ;
#5268 = CARTESIAN_POINT ( 'NONE',  ( 0.3412792617076850221, 0.05967164814832588010, 0.1377952755905512139 ) ) ;
#5269 = B_SPLINE_CURVE_WITH_KNOTS ( 'NONE', 3,
 ( #4914, #26253, #829, #13527, #7317, #22432 ),
 .UNSPECIFIED., .F., .F.,
 ( 4, 2, 4 ),
 ( 0.000000000000000000, 0.2500000000000000000, 0.5000000000000000000 ),
 .UNSPECIFIED. ) ;
#5270 = DIRECTION ( 'NONE',  ( -1.000000000000000000, 0.000000000000000000, 0.000000000000000000 ) ) ;
#5271 = ORIENTED_EDGE ( 'NONE', *, *, #9231, .T. ) ;
#5272 = CARTESIAN_POINT ( 'NONE',  ( -0.3075317527319259558, 0.1775220790475501298, 1.953740157480314821 ) ) ;
#5273 = ORIENTED_EDGE ( 'NONE', *, *, #11599, .T. ) ;
#5274 = CARTESIAN_POINT ( 'NONE',  ( -0.3599896729929590866, -0.2761764805255594313, -1.934055118110236338 ) ) ;
#5275 = DIRECTION ( 'NONE',  ( 0.000000000000000000, 1.000000000000000000, 0.000000000000000000 ) ) ;
#5276 = DIRECTION ( 'NONE',  ( 0.000000000000000000, -1.000000000000000000, 0.000000000000000000 ) ) ;
#5277 = CARTESIAN_POINT ( 'NONE',  ( -0.01298392085634582534, 0.3147567063785114416, -3.174859699051844064 ) ) ;
#5278 = DIRECTION ( 'NONE',  ( -0.9790454724845842893, -0.1018208755700880375, 0.1763589297585410332 ) ) ;
#5279 = CARTESIAN_POINT ( 'NONE',  ( -0.7874015748031496509, 0.7427623301578110127, -0.4227432117344842588 ) ) ;
#5280 = VERTEX_POINT ( 'NONE', #20765 ) ;
#5281 = DIRECTION ( 'NONE',  ( -1.000000000000000000, 0.000000000000000000, 0.000000000000000000 ) ) ;
#5282 = CARTESIAN_POINT ( 'NONE',  ( -0.2089723435111595085, -0.4324731448915372645, 0.2194422276631042279 ) ) ;
#5283 = ORIENTED_EDGE ( 'NONE', *, *, #17027, .F. ) ;
#5284 = CARTESIAN_POINT ( 'NONE',  ( 0.1886891683788910479, -0.3267488823401750730, -3.100567304031762284 ) ) ;
#5285 = CARTESIAN_POINT ( 'NONE',  ( 0.000000000000000000, 0.000000000000000000, 0.2755905511811023723 ) ) ;
#5286 = DIRECTION ( 'NONE',  ( 0.000000000000000000, 1.000000000000000000, 0.000000000000000000 ) ) ;
#5287 = VERTEX_POINT ( 'NONE', #22741 ) ;
#5288 = CARTESIAN_POINT ( 'NONE',  ( -0.4498374011142775575, 0.05926487674658489219, -1.934055118110236338 ) ) ;
#5289 = B_SPLINE_CURVE_WITH_KNOTS ( 'NONE', 3,
 ( #27178, #13745, #7819, #5559 ),
 .UNSPECIFIED., .F., .F.,
 ( 4, 4 ),
 ( 0.000000000000000000, 1.199999999999999956 ),
 .UNSPECIFIED. ) ;
#5290 = EDGE_CURVE ( 'NONE', #8047, #17815, #15314, .T. ) ;
#5291 = TOROIDAL_SURFACE ( 'NONE', #19744, 0.5610236220472440971, 0.1003937007874015908 ) ;
#5292 = ORIENTED_EDGE ( 'NONE', *, *, #19478, .F. ) ;
#5293 = ORIENTED_EDGE ( 'NONE', *, *, #21682, .F. ) ;
#5294 = VECTOR ( 'NONE', #1675, 39.37007874015748143 ) ;
#5295 = CARTESIAN_POINT ( 'NONE',  ( -0.4280150452258433269, -0.5303309585532346437, -0.4308570359575180642 ) ) ;
#5296 = DIRECTION ( 'NONE',  ( 1.000000000000000000, 0.000000000000000000, 0.000000000000000000 ) ) ;
#5297 = CARTESIAN_POINT ( 'NONE',  ( -0.03349795313264326141, 0.5118110236220472231, 1.747047244094488194 ) ) ;
#5298 = ORIENTED_EDGE ( 'NONE', *, *, #26389, .T. ) ;
#5299 = SURFACE_SIDE_STYLE ('',( #18275 ) ) ;
#5300 = ORIENTED_EDGE ( 'NONE', *, *, #1608, .F. ) ;
#5301 = ORIENTED_EDGE ( 'NONE', *, *, #1249, .F. ) ;
#5302 = CARTESIAN_POINT ( 'NONE',  ( -0.3267488823401750730, -0.1886891683788910756, -3.100567304031762284 ) ) ;
#5303 = CARTESIAN_POINT ( 'NONE',  ( -0.6130487771524342211, 1.107101695598143642, -0.07148403028289961048 ) ) ;
#5304 = ( REPRESENTATION_RELATIONSHIP ('NONE','NONE', #12434, #24703 ) REPRESENTATION_RELATIONSHIP_WITH_TRANSFORMATION ( #7765 )SHAPE_REPRESENTATION_RELATIONSHIP( ) ) ;
#5305 = FACE_OUTER_BOUND ( 'NONE', #4175, .T. ) ;
#5306 = CARTESIAN_POINT ( 'NONE',  ( -0.01288382760289888754, 0.2165354330708661457, -3.646653543307086576 ) ) ;
#5307 = ORIENTED_EDGE ( 'NONE', *, *, #15668, .T. ) ;
#5308 = ORIENTED_EDGE ( 'NONE', *, *, #15428, .F. ) ;
#5309 = CARTESIAN_POINT ( 'NONE',  ( 0.2564173815262089096, 0.4442189740295122147, -1.550196850393701364 ) ) ;
#5310 = DIRECTION ( 'NONE',  ( 0.000000000000000000, 0.000000000000000000, 1.000000000000000000 ) ) ;
#5311 = CARTESIAN_POINT ( 'NONE',  ( -0.8725268807032540153, 0.000000000000000000, -1.052618110236220428 ) ) ;
#5312 = VERTEX_POINT ( 'NONE', #23330 ) ;
#5313 = CARTESIAN_POINT ( 'NONE',  ( 0.1970259548082060608, 0.3996230174612934172, -1.934055118110236338 ) ) ;
#5314 = EDGE_CURVE ( 'NONE', #21174, #27329, #26114, .T. ) ;
#5315 = LINE ( 'NONE', #20291, #27238 ) ;
#5316 = DIRECTION ( 'NONE',  ( -0.9848077530122079093, 0.1736481776669309696, 0.000000000000000000 ) ) ;
#5317 = EDGE_CURVE ( 'NONE', #9496, #3844, #5760, .T. ) ;
#5318 = VECTOR ( 'NONE', #11192, 39.37007874015748143 ) ;
#5319 = FACE_OUTER_BOUND ( 'NONE', #18999, .T. ) ;
#5321 = CARTESIAN_POINT ( 'NONE',  ( 0.000000000000000000, 0.000000000000000000, 1.953740157480315043 ) ) ;
#5322 = AXIS2_PLACEMENT_3D ( 'NONE', #12761, #14484, #20963 ) ;
#5323 = CARTESIAN_POINT ( 'NONE',  ( 0.03532354024591842501, -0.6299212598425196763, 0.000000000000000000 ) ) ;
#5324 = DIRECTION ( 'NONE',  ( 0.000000000000000000, 0.000000000000000000, -1.000000000000000000 ) ) ;
#5325 = PRODUCT_DEFINITION_SHAPE ( 'NONE', 'NONE',  #27916 ) ;
#5326 = DIRECTION ( 'NONE',  ( 0.000000000000000000, -1.000000000000000000, 0.000000000000000000 ) ) ;
#5327 = EDGE_CURVE ( 'NONE', #4135, #218, #13931, .T. ) ;
#5328 = DIRECTION ( 'NONE',  ( -0.000000000000000000, -1.000000000000000000, -0.000000000000000000 ) ) ;
#5330 = CARTESIAN_POINT ( 'NONE',  ( -0.1775730735577452091, -0.3074993854542726335, 1.953740157480315043 ) ) ;
#5329 = AXIS2_PLACEMENT_3D ( 'NONE', #24038, #4675, #11179 ) ;
#5331 = ORIENTED_EDGE ( 'NONE', *, *, #10267, .F. ) ;
#5332 = CARTESIAN_POINT ( 'NONE',  ( 0.6882266799383700562, -0.2663285262597259728, -0.2694682288251842861 ) ) ;
#5333 = CARTESIAN_POINT ( 'NONE',  ( -0.3338887748335570560, -1.269220122646561588, -0.8285976369166339062 ) ) ;
#5334 = CARTESIAN_POINT ( 'NONE',  ( 0.1755067523729419432, 0.6057501678605275997, 0.000000000000000000 ) ) ;
#5335 = CARTESIAN_POINT ( 'NONE',  ( -0.5043504886477528926, -0.1712563538833036247, 1.747047244094488194 ) ) ;
#5336 = CARTESIAN_POINT ( 'NONE',  ( -0.3121994997598287469, 0.4069448477556107946, 1.766732283464566899 ) ) ;
#5337 = AXIS2_PLACEMENT_3D ( 'NONE', #20855, #16478, #18575 ) ;
#5338 = ORIENTED_EDGE ( 'NONE', *, *, #24560, .T. ) ;
#5339 = VECTOR ( 'NONE', #18152, 39.37007874015748143 ) ;
#5340 = CARTESIAN_POINT ( 'NONE',  ( -0.09139240964747702423, 0.07874015748031500117, -1.981023540891279271E-18 ) ) ;
#5341 = EDGE_LOOP ( 'NONE', ( #21168, #1185, #24144, #3614 ) ) ;
#5342 = CARTESIAN_POINT ( 'NONE',  ( -0.09139240964747702423, 0.07874015748031500117, -1.981023540891279271E-18 ) ) ;
#5343 = CARTESIAN_POINT ( 'NONE',  ( -0.07217847769028858107, 0.04546065111729338110, 0.000000000000000000 ) ) ;
#5344 = CARTESIAN_POINT ( 'NONE',  ( -0.3996230174612752095, 0.1970259548082017587, -1.934055118110236338 ) ) ;
#5345 = VERTEX_POINT ( 'NONE', #10295 ) ;
#5346 = CARTESIAN_POINT ( 'NONE',  ( 0.3346456692913385988, 0.000000000000000000, 1.973425196850393970 ) ) ;
#5347 = ORIENTED_EDGE ( 'NONE', *, *, #6996, .F. ) ;
#5348 = ORIENTED_EDGE ( 'NONE', *, *, #9549, .T. ) ;
#5349 = CARTESIAN_POINT ( 'NONE',  ( 0.4669911931914907388, -0.1585706980422228185, -1.569881889763779625 ) ) ;
#5350 = CIRCLE ( 'NONE', #9865, 0.8267716535433071723 ) ;
#5351 = ORIENTED_EDGE ( 'NONE', *, *, #9973, .F. ) ;
#5352 = VERTEX_POINT ( 'NONE', #25425 ) ;
#5353 = ADVANCED_FACE ( 'NONE', ( #6089, #12977 ), #14853, .T. ) ;
#5354 = DIRECTION ( 'NONE',  ( -0.2036417511401758251, 0.4895227362422921447, -0.8478782506317885659 ) ) ;
#5355 = CONTEXT_DEPENDENT_SHAPE_REPRESENTATION ( #5865, #4847 ) ;
#5356 = CARTESIAN_POINT ( 'NONE',  ( 0.000000000000000000, 0.7283464566929134243, 0.01181102362204724393 ) ) ;
#5357 = ADVANCED_FACE ( 'NONE', ( #4767 ), #2650, .T. ) ;
#5358 = CARTESIAN_POINT ( 'NONE',  ( 0.000000000000000000, 0.000000000000000000, -0.05511811023622047168 ) ) ;
#5359 = CARTESIAN_POINT ( 'NONE',  ( 0.5378064472801062923, -0.3110113600220468233, 0.09684874924366436433 ) ) ;
#5360 = CARTESIAN_POINT ( 'NONE',  ( -0.6116756676109479374, 0.7064581683589515881, 0.02937168582378947568 ) ) ;
#5361 = LINE ( 'NONE', #5212, #18750 ) ;
#5362 = EDGE_CURVE ( 'NONE', #24896, #5769, #7155, .T. ) ;
#5363 = CIRCLE ( 'NONE', #851, 0.01181102362204754924 ) ;
#5364 = CARTESIAN_POINT ( 'NONE',  ( 0.000000000000000000, 0.000000000000000000, -4.330708661396418080 ) ) ;
#5365 = ADVANCED_FACE ( 'NONE', ( #9008, #17761 ), #11685, .T. ) ;
#5366 = AXIS2_PLACEMENT_3D ( 'NONE', #1302, #7513, #9908 ) ;
#5367 = CARTESIAN_POINT ( 'NONE',  ( -0.2211428102655905170, 0.2521176338356723168, 1.953740157480315043 ) ) ;
#5368 = UNCERTAINTY_MEASURE_WITH_UNIT (LENGTH_MEASURE( 1.000000000000000082E-05 ), #4839, 'distance_accuracy_value', 'NONE') ;
#5369 = ORIENTED_EDGE ( 'NONE', *, *, #24366, .T. ) ;
#5370 = DIRECTION ( 'NONE',  ( 0.000000000000000000, 0.000000000000000000, 1.000000000000000000 ) ) ;
#5371 = CARTESIAN_POINT ( 'NONE',  ( -0.1968503937007874127, -1.092519685039370136, 0.000000000000000000 ) ) ;
#5372 = CARTESIAN_POINT ( 'NONE',  ( -6.518592411209533944E-17, -0.5322834645669292097, 0.06614173228346456601 ) ) ;
#5373 = DIRECTION ( 'NONE',  ( 0.000000000000000000, 1.000000000000000000, 0.000000000000000000 ) ) ;
#5374 = AXIS2_PLACEMENT_3D ( 'NONE', #16718, #2019, #27604 ) ;
#5375 = DIRECTION ( 'NONE',  ( 0.000000000000000000, 0.000000000000000000, 1.000000000000000000 ) ) ;
#5376 = FACE_OUTER_BOUND ( 'NONE', #5601, .T. ) ;
#5377 = DIRECTION ( 'NONE',  ( -0.000000000000000000, 1.000000000000000000, -0.000000000000000000 ) ) ;
#5378 = ORIENTED_EDGE ( 'NONE', *, *, #23846, .T. ) ;
#5379 = DIRECTION ( 'NONE',  ( -1.000000000000000000, 0.000000000000000000, 0.000000000000000000 ) ) ;
#5380 = CIRCLE ( 'NONE', #23912, 0.7500000000000001110 ) ;
#5381 = ORIENTED_EDGE ( 'NONE', *, *, #15398, .T. ) ;
#5382 = AXIS2_PLACEMENT_3D ( 'NONE', #3250, #26145, #11165 ) ;
#5383 = CARTESIAN_POINT ( 'NONE',  ( -9.069736220472440932E-16, -0.8267716535433070613, 0.7883858267716535861 ) ) ;
#5384 = DIRECTION ( 'NONE',  ( 0.000000000000000000, 0.000000000000000000, 1.000000000000000000 ) ) ;
#5385 = CIRCLE ( 'NONE', #8927, 0.5322834645669292097 ) ;
#5386 = CARTESIAN_POINT ( 'NONE',  ( -0.07870736599817637624, 0.1968503937007873850, -3.608715228723573976 ) ) ;
#5387 = VERTEX_POINT ( 'NONE', #24671 ) ;
#5388 = CARTESIAN_POINT ( 'NONE',  ( 0.7283464566929135353, 0.000000000000000000, 0.3425196850393700809 ) ) ;
#5389 = EDGE_LOOP ( 'NONE', ( #10548, #6140, #22300, #27754, #5059, #10387, #9766, #7521 ) ) ;
#5390 = EDGE_CURVE ( 'NONE', #6287, #14933, #26379, .T. ) ;
#5391 = CARTESIAN_POINT ( 'NONE',  ( -0.2195865873860579631, -0.6052790189093463225, 0.1183902030410438760 ) ) ;
#5392 = FACE_OUTER_BOUND ( 'NONE', #16212, .T. ) ;
#5393 = CARTESIAN_POINT ( 'NONE',  ( 0.7871730179869745880, 0.4038169352867496120, 0.1713250154738354125 ) ) ;
#5394 = ADVANCED_FACE ( 'NONE', ( #964 ), #8509, .T. ) ;
#5395 = DIRECTION ( 'NONE',  ( 1.000000000000000000, 0.000000000000000000, 0.000000000000000000 ) ) ;
#5396 = CARTESIAN_POINT ( 'NONE',  ( 0.09590060490395689585, -0.1136516277932324709, -0.1968503937007874127 ) ) ;
#5397 = EDGE_LOOP ( 'NONE', ( #10780, #27110 ) ) ;
#5398 = CARTESIAN_POINT ( 'NONE',  ( 0.08676778863010990717, 0.3239425792934408910, 1.973425196850393970 ) ) ;
#5399 = CARTESIAN_POINT ( 'NONE',  ( 0.3252100150720381722, -0.3707612262533039327, -1.550196850393700920 ) ) ;
#5400 = VECTOR ( 'NONE', #9652, 39.37007874015748143 ) ;
#5401 = DIRECTION ( 'NONE',  ( -0.000000000000000000, 1.000000000000000000, -0.000000000000000000 ) ) ;
#5402 = CARTESIAN_POINT ( 'NONE',  ( -0.3338887748335582772, -9.254566434370079157E-06, -2.341456692880161228 ) ) ;
#5403 = CARTESIAN_POINT ( 'NONE',  ( -0.5476281405333195407, -0.07214854559197286799, 0.9202755905511811330 ) ) ;
#5404 = DIRECTION ( 'NONE',  ( 1.000000000000000000, 0.000000000000000000, 0.000000000000000000 ) ) ;
#5405 = FACE_OUTER_BOUND ( 'NONE', #5739, .T. ) ;
#5406 = ORIENTED_EDGE ( 'NONE', *, *, #22612, .T. ) ;
#5407 = CARTESIAN_POINT ( 'NONE',  ( 0.1490609433615240342, 0.2393035190771456711, 0.4144858534716441278 ) ) ;
#5408 = CARTESIAN_POINT ( 'NONE',  ( -0.1275996891957758561, 0.4763861460130329184, -1.569881889763779625 ) ) ;
#5409 = DIRECTION ( 'NONE',  ( 0.000000000000000000, 0.000000000000000000, 1.000000000000000000 ) ) ;
#5410 = CARTESIAN_POINT ( 'NONE',  ( 0.03532354024591839031, -0.07677165354330710290, 0.000000000000000000 ) ) ;
#5411 = CARTESIAN_POINT ( 'NONE',  ( 0.2158067241000556635, -0.4466421405284947688, 0.1734435148016537642 ) ) ;
#5412 = SPHERICAL_SURFACE ( 'NONE', #20826, 0.1003956692913385851 ) ;
#5413 = CARTESIAN_POINT ( 'NONE',  ( 0.2311492806687369950, -0.4794744477484330636, 0.1322810039474933141 ) ) ;
#5414 = ORIENTED_EDGE ( 'NONE', *, *, #27515, .F. ) ;
#5415 = SHAPE_REPRESENTATION ( 'O-Ring 36.5x2.65', ( #11588 ), #12073 ) ;
#5416 = B_SPLINE_CURVE_WITH_KNOTS ( 'NONE', 3,
 ( #9422, #22582, #24831, #12123, #9719, #18320 ),
 .UNSPECIFIED., .F., .F.,
 ( 4, 2, 4 ),
 ( 0.000000000000000000, 0.2500000000000000000, 0.5000000000000000000 ),
 .UNSPECIFIED. ) ;
#5417 = CARTESIAN_POINT ( 'NONE',  ( 0.9842519685039370358, -0.1525590551181102428, 0.2952755905511810774 ) ) ;
#5418 = DIRECTION ( 'NONE',  ( 0.9848077530122081313, 0.1736481776669299981, -0.000000000000000000 ) ) ;
#5419 = DIRECTION ( 'NONE',  ( 1.000000000000000000, 0.000000000000000000, 0.000000000000000000 ) ) ;
#5420 = EDGE_LOOP ( 'NONE', ( #26664, #25848 ) ) ;
#5421 = CIRCLE ( 'NONE', #21220, 0.02362204724409448786 ) ;
#5422 = CARTESIAN_POINT ( 'NONE',  ( -0.02325127328499143609, 0.3543292900372674303, 1.953740157480315043 ) ) ;
#5423 = VERTEX_POINT ( 'NONE', #20161 ) ;
#5424 = EDGE_CURVE ( 'NONE', #20128, #6015, #2513, .T. ) ;
#5425 = CARTESIAN_POINT ( 'NONE',  ( -0.4296318976989931815, -0.1458850421962362698, -1.934055118110236338 ) ) ;
#5426 = DIRECTION ( 'NONE',  ( 0.000000000000000000, 0.000000000000000000, -1.000000000000000000 ) ) ;
#5427 = CARTESIAN_POINT ( 'NONE',  ( 0.1504778549385457909, -0.2746646418458098537, -0.4002635090060460699 ) ) ;
#5428 = CARTESIAN_POINT ( 'NONE',  ( -0.3268939675028499914, -0.1881330340946393564, 0.1992125984251968684 ) ) ;
#5429 = CARTESIAN_POINT ( 'NONE',  ( 0.4858607088160724063, -0.2805118110236220486, 0.2775610236220472093 ) ) ;
#5430 = ORIENTED_EDGE ( 'NONE', *, *, #2909, .F. ) ;
#5431 = CARTESIAN_POINT ( 'NONE',  ( -0.03532354024591901481, -0.8267716535433070613, 0.8267716535433070613 ) ) ;
#5432 = B_SPLINE_CURVE_WITH_KNOTS ( 'NONE', 3,
 ( #957, #10251, #17186, #16914, #3908, #21143 ),
 .UNSPECIFIED., .F., .F.,
 ( 4, 1, 1, 4 ),
 ( 0.000000000000000000, 0.4285714285714292138, 0.7142857142857154118, 1.000000000000000000 ),
 .UNSPECIFIED. ) ;
#5433 = ADVANCED_FACE ( 'NONE', ( #7173 ), #21880, .F. ) ;
#5434 = EDGE_LOOP ( 'NONE', ( #1497, #47, #6439, #12 ) ) ;
#5435 = DIRECTION ( 'NONE',  ( -1.224646799147353207E-16, 1.000000000000000000, 0.000000000000000000 ) ) ;
#5436 = AXIS2_PLACEMENT_3D ( 'NONE', #12609, #23216, #27733 ) ;
#5437 = DIRECTION ( 'NONE',  ( 0.000000000000000000, 0.000000000000000000, 1.000000000000000000 ) ) ;
#5438 = ORIENTED_EDGE ( 'NONE', *, *, #9660, .T. ) ;
#5439 = CARTESIAN_POINT ( 'NONE',  ( -0.2296683860596777926, -0.2993674444872276297, -3.100567304031764060 ) ) ;
#5440 = CARTESIAN_POINT ( 'NONE',  ( -0.3460488714339713390, -0.09275962632023325438, -3.115157480314960647 ) ) ;
#5441 = UNCERTAINTY_MEASURE_WITH_UNIT (LENGTH_MEASURE( 1.000000000000000082E-05 ), #19, 'distance_accuracy_value', 'NONE') ;
#5442 = ORIENTED_EDGE ( 'NONE', *, *, #7200, .T. ) ;
#5443 = CARTESIAN_POINT ( 'NONE',  ( -0.2991932138496531390, 0.3411003281196664516, -1.934055118110236338 ) ) ;
#5444 = PRODUCT_CONTEXT ( 'NONE', #9969, 'mechanical' ) ;
#5445 = CARTESIAN_POINT ( 'NONE',  ( -0.7635713814939685262, 0.2506761191097937047, -0.2749095812957952911 ) ) ;
#5446 = AXIS2_PLACEMENT_3D ( 'NONE', #4082, #10991, #26103 ) ;
#5447 = ORIENTED_EDGE ( 'NONE', *, *, #15874, .F. ) ;
#5448 = CARTESIAN_POINT ( 'NONE',  ( -0.3503688343903059166, -1.019241955546190903, -0.5558691273266149757 ) ) ;
#5449 = CARTESIAN_POINT ( 'NONE',  ( 0.000000000000000000, 0.000000000000000000, -0.04133858267716535029 ) ) ;
#5450 = CARTESIAN_POINT ( 'NONE',  ( 0.5043504886477625515, 0.1712563538832952981, 1.747047244094488194 ) ) ;
#5451 = ORIENTED_EDGE ( 'NONE', *, *, #16037, .T. ) ;
#5452 = EDGE_LOOP ( 'NONE', ( #15442, #19741 ) ) ;
#5453 = PRESENTATION_LAYER_ASSIGNMENT (  '', '', ( #2724 ) ) ;
#5454 = CARTESIAN_POINT ( 'NONE',  ( 0.3572819248074489140, -0.1213180142433802344, -3.100567304031756066 ) ) ;
#5455 = ORIENTED_EDGE ( 'NONE', *, *, #18104, .T. ) ;
#5456 = CARTESIAN_POINT ( 'NONE',  ( 0.000000000000000000, 0.000000000000000000, -0.2480314960629921295 ) ) ;
#5457 = CARTESIAN_POINT ( 'NONE',  ( 0.2938622683360631593, 0.000000000000000000, -3.745078740157480546 ) ) ;
#5458 = EDGE_LOOP ( 'NONE', ( #21728, #2377, #20398, #4775, #12744 ) ) ;
#5459 = DIRECTION ( 'NONE',  ( 0.000000000000000000, 0.000000000000000000, -1.000000000000000000 ) ) ;
#5460 = ORIENTED_EDGE ( 'NONE', *, *, #14509, .F. ) ;
#5461 = ORIENTED_EDGE ( 'NONE', *, *, #2070, .F. ) ;
#5462 = ORIENTED_EDGE ( 'NONE', *, *, #20086, .F. ) ;
#5463 = CARTESIAN_POINT ( 'NONE',  ( -0.6806799598997224088, 0.08941145402117105234, 0.2332800728132976564 ) ) ;
#5464 = CARTESIAN_POINT ( 'NONE',  ( 0.000000000000000000, 0.000000000000000000, -0.2204724409448818867 ) ) ;
#5465 = EDGE_CURVE ( 'NONE', #280, #9781, #24261, .T. ) ;
#5466 = CARTESIAN_POINT ( 'NONE',  ( -0.2490711204941342405, 1.060861271878683176, -0.6594961294738858060 ) ) ;
#5467 = CARTESIAN_POINT ( 'NONE',  ( -0.07214943758244271588, -0.5511811023622046335, 0.9202755905511812440 ) ) ;
#5468 = CARTESIAN_POINT ( 'NONE',  ( 0.3259357382551449356, 0.08759279594700336569, 1.973425196850393970 ) ) ;
#5469 = FACE_OUTER_BOUND ( 'NONE', #13610, .T. ) ;
#5470 = AXIS2_PLACEMENT_3D ( 'NONE', #12945, #21439, #4479 ) ;
#5471 = CIRCLE ( 'NONE', #19017, 0.6212598425196850238 ) ;
#5472 = EDGE_CURVE ( 'NONE', #10266, #9518, #21080, .T. ) ;
#5473 = DIRECTION ( 'NONE',  ( -1.000000000000000000, 0.000000000000000000, 0.000000000000000000 ) ) ;
#5474 = CARTESIAN_POINT ( 'NONE',  ( -0.3661417322834645272, 0.9448818897637796255, -0.1082677165354330867 ) ) ;
#5475 = ORIENTED_EDGE ( 'NONE', *, *, #19235, .T. ) ;
#5476 = CARTESIAN_POINT ( 'NONE',  ( 0.4858607088160724063, -0.2805118110236220486, 0.1771653543307086520 ) ) ;
#5477 = DIRECTION ( 'NONE',  ( -1.000000000000000000, 0.000000000000000000, 0.000000000000000000 ) ) ;
#5478 = EDGE_LOOP ( 'NONE', ( #6416, #14959, #835, #13822 ) ) ;
#5479 = DIRECTION ( 'NONE',  ( -0.5000000000000001110, 0.8660254037844384856, 0.000000000000000000 ) ) ;
#5480 = ORIENTED_EDGE ( 'NONE', *, *, #1724, .T. ) ;
#5481 = CARTESIAN_POINT ( 'NONE',  ( 0.3065394984574514314, 0.3644188803065985249, 0.2330651858034864243 ) ) ;
#5482 = CARTESIAN_POINT ( 'NONE',  ( 0.7874015748031496509, -0.6060691875862894706, 0.08482860590294842573 ) ) ;
#5483 = CARTESIAN_POINT ( 'NONE',  ( 0.4600326175560532915, -0.2268096725222599475, 1.747047244094488194 ) ) ;
#5484 = APPLICATION_CONTEXT ( 'automotive_design' ) ;
#5485 = CARTESIAN_POINT ( 'NONE',  ( -0.07874015748031502893, 0.1968503937007874127, -3.272637795275590733 ) ) ;
#5486 = B_SPLINE_CURVE_WITH_KNOTS ( 'NONE', 3,
 ( #9797, #13752, #15872, #5129, #20252, #914, #1196, #14193, #22795, #3419, #16021, #12057, #24619, #22517, #5277, #20676, #13898, #1056, #25186, #10629, #21243, #5714, #27747, #8246, #20812, #27318 ),
 .UNSPECIFIED., .F., .F.,
 ( 4, 2, 2, 2, 2, 2, 2, 2, 2, 2, 2, 2, 4 ),
 ( -0.006894309973022127655, -0.006402040495999860442, -0.005909771018977594097, -0.004925232064933059671, -0.003940693110888525245, -0.003448423633866250226, -0.002956154156843975207, -0.002463884679821699321, -0.001971615202799424302, -0.0009870762487548898761, -2.537294710355450511E-06, 0.0004897321823118935477, 0.0009820016593341408112 ),
 .UNSPECIFIED. ) ;
#5487 = CARTESIAN_POINT ( 'NONE',  ( 0.1327036767659691974, 0.4954415918531168139, 1.747047244094488194 ) ) ;
#5488 = ADVANCED_FACE ( 'NONE', ( #4909 ), #13663, .F. ) ;
#5489 = VERTEX_POINT ( 'NONE', #18159 ) ;
#5490 = CARTESIAN_POINT ( 'NONE',  ( 1.877524803149606209E-16, 5.303588500244442984E-17, -0.4330708661417322913 ) ) ;
#5491 = ORIENTED_EDGE ( 'NONE', *, *, #544, .T. ) ;
#5492 = CARTESIAN_POINT ( 'NONE',  ( 0.6709908451338839619, -0.1528902114222553399, 0.3401599409343967761 ) ) ;
#5493 = ( NAMED_UNIT ( * ) PLANE_ANGLE_UNIT ( ) SI_UNIT ( $, .RADIAN. ) ) ;
#5494 = CARTESIAN_POINT ( 'NONE',  ( 0.1522836969735573143, -0.4909267390297480382, 0.05591742528025181458 ) ) ;
#5495 = FACE_OUTER_BOUND ( 'NONE', #9560, .T. ) ;
#5496 = ORIENTED_EDGE ( 'NONE', *, *, #25810, .T. ) ;
#5497 = CIRCLE ( 'NONE', #5034, 0.4786070381542913421 ) ;
#5498 = EDGE_LOOP ( 'NONE', ( #16715, #23392, #1461, #22477 ) ) ;
#5499 = MECHANICAL_DESIGN_GEOMETRIC_PRESENTATION_REPRESENTATION (  '', ( #27617 ), #17674 ) ;
#5500 = CARTESIAN_POINT ( 'NONE',  ( 0.4669911931914765835, 0.1585706980422571244, -1.569881889763779625 ) ) ;
#5501 = EDGE_CURVE ( 'NONE', #2628, #8924, #18353, .T. ) ;
#5502 = ORIENTED_EDGE ( 'NONE', *, *, #1800, .F. ) ;
#5503 = ORIENTED_EDGE ( 'NONE', *, *, #23744, .F. ) ;
#5504 = ORIENTED_EDGE ( 'NONE', *, *, #11101, .T. ) ;
#5505 = DIRECTION ( 'NONE',  ( 0.000000000000000000, 0.000000000000000000, 1.000000000000000000 ) ) ;
#5506 = CARTESIAN_POINT ( 'NONE',  ( -0.1718374205099799101, -0.4703827404237102550, 0.2574803149606298969 ) ) ;
#5507 = DIRECTION ( 'NONE',  ( -1.000000000000000000, 0.000000000000000000, 0.000000000000000000 ) ) ;
#5508 = CARTESIAN_POINT ( 'NONE',  ( -0.4798812372167962081, 0.4571014508549643973, 0.1560354075451796108 ) ) ;
#5509 = DIRECTION ( 'NONE',  ( 0.000000000000000000, 0.000000000000000000, 1.000000000000000000 ) ) ;
#5510 = PRODUCT ( 'O-Ring 26.5x2.65', 'O-Ring 26.5x2.65', '', ( #21672 ) ) ;
#5511 = AXIS2_PLACEMENT_3D ( 'NONE', #8109, #25334, #5997 ) ;
#5512 = ORIENTED_EDGE ( 'NONE', *, *, #15471, .T. ) ;
#5513 = CARTESIAN_POINT ( 'NONE',  ( 0.4681308612729632168, -0.1074986424507603650, 0.2529987172375934845 ) ) ;
#5514 = CARTESIAN_POINT ( 'NONE',  ( 0.0003454908279976030448, 0.3771652360013086347, 0.07637630750536809898 ) ) ;
#5515 = VECTOR ( 'NONE', #11484, 39.37007874015748854 ) ;
#5516 = CARTESIAN_POINT ( 'NONE',  ( -0.4921259842519685179, 0.06441914069860968373, -1.569881889763779625 ) ) ;
#5517 = CARTESIAN_POINT ( 'NONE',  ( -9.160727710493059047E-17, 0.000000000000000000, -0.02362204724409468909 ) ) ;
#5518 = EDGE_CURVE ( 'NONE', #27249, #6246, #11221, .T. ) ;
#5519 = ORIENTED_EDGE ( 'NONE', *, *, #12634, .F. ) ;
#5520 = ORIENTED_EDGE ( 'NONE', *, *, #2947, .T. ) ;
#5521 = B_SPLINE_CURVE_WITH_KNOTS ( 'NONE', 3,
 ( #10894, #19509, #9040, #4539, #26275, #26010 ),
 .UNSPECIFIED., .F., .F.,
 ( 4, 2, 4 ),
 ( 0.2291966065698859967, 0.2305109203526899964, 0.2318252341354939960 ),
 .UNSPECIFIED. ) ;
#5522 = EDGE_CURVE ( 'NONE', #26797, #21888, #18883, .T. ) ;
#5523 = CIRCLE ( 'NONE', #20464, 0.4606299212598425341 ) ;
#5524 = VERTEX_POINT ( 'NONE', #22146 ) ;
#5525 = AXIS2_PLACEMENT_3D ( 'NONE', #12862, #21491, #2133 ) ;
#5526 = CARTESIAN_POINT ( 'NONE',  ( -0.3294268239828485600, 0.000000000000000000, -0.1625845656552793450 ) ) ;
#5527 = EDGE_CURVE ( 'NONE', #24760, #25529, #17543, .T. ) ;
#5528 = CARTESIAN_POINT ( 'NONE',  ( 0.6299212598425196763, 0.000000000000000000, 0.000000000000000000 ) ) ;
#5529 = CARTESIAN_POINT ( 'NONE',  ( 0.07874015747999514592, 0.1968503937007873850, -3.558537267005753346 ) ) ;
#5530 = VERTEX_POINT ( 'NONE', #19268 ) ;
#5531 = ORIENTED_EDGE ( 'NONE', *, *, #2574, .T. ) ;
#5532 = VECTOR ( 'NONE', #13554, 39.37007874015748143 ) ;
#5533 = CARTESIAN_POINT ( 'NONE',  ( 0.6299212598425196763, 0.4807043897637795493, 0.000000000000000000 ) ) ;
#5534 = CARTESIAN_POINT ( 'NONE',  ( -0.1968503937007874127, -0.07874015748031495954, 0.04546065111729338803 ) ) ;
#5535 = CARTESIAN_POINT ( 'NONE',  ( 0.3289909311256232205, 0.1896185148830506484, -3.100567304031764060 ) ) ;
#5536 = CARTESIAN_POINT ( 'NONE',  ( -0.4980314960629921295, 0.000000000000000000, -6.010066929133858501E-17 ) ) ;
#5537 = CARTESIAN_POINT ( 'NONE',  ( 0.7871730179869350641, 0.2557924603611196890, -0.2773276354978094771 ) ) ;
#5538 = VERTEX_POINT ( 'NONE', #18305 ) ;
#5539 = CARTESIAN_POINT ( 'NONE',  ( -0.3324885138898245329, -0.04380447413658584976, 1.973425196850393970 ) ) ;
#5540 = DIRECTION ( 'NONE',  ( 0.000000000000000000, 1.000000000000000000, 0.000000000000000000 ) ) ;
#5541 = CONICAL_SURFACE ( 'NONE', #13632, 0.1106489370078740098, 0.08726646250000029414 ) ;
#5542 = DIRECTION ( 'NONE',  ( 0.000000000000000000, 1.000000000000000000, 0.000000000000000000 ) ) ;
#5543 = CARTESIAN_POINT ( 'NONE',  ( -0.08582677165393072516, 0.000000000000000000, -0.4724409448841456749 ) ) ;
#5544 = VERTEX_POINT ( 'NONE', #26952 ) ;
#5545 = CARTESIAN_POINT ( 'NONE',  ( -0.4160174684701755665, 0.3320469875258716397, 0.3401599409343964431 ) ) ;
#5546 = EDGE_CURVE ( 'NONE', #22287, #8702, #10647, .T. ) ;
#5547 = CARTESIAN_POINT ( 'NONE',  ( 0.4763861460130340286, 0.1275996891957706103, -1.569881889763779625 ) ) ;
#5548 = TOROIDAL_SURFACE ( 'NONE', #20874, 0.7883858267716535861, 0.05216535433070866590 ) ;
#5549 = DIRECTION ( 'NONE',  ( 1.000000000000000000, 0.000000000000000000, 0.000000000000000000 ) ) ;
#5550 = CARTESIAN_POINT ( 'NONE',  ( -0.3937007874015748254, 4.821444091131312140E-17, -3.036417322828325105 ) ) ;
#5551 = LINE ( 'NONE', #27693, #25826 ) ;
#5552 = EDGE_CURVE ( 'NONE', #23745, #23749, #5363, .T. ) ;
#5553 = FACE_OUTER_BOUND ( 'NONE', #27528, .T. ) ;
#5554 = ORIENTED_EDGE ( 'NONE', *, *, #14924, .F. ) ;
#5555 = EDGE_LOOP ( 'NONE', ( #8348, #21160, #7773, #25328, #21358, #1713 ) ) ;
#5556 = DIRECTION ( 'NONE',  ( -0.9236347588935202024, 0.3832738344365670957, 0.000000000000000000 ) ) ;
#5557 = FACE_BOUND ( 'NONE', #11418, .T. ) ;
#5558 = PRODUCT_DEFINITION_SHAPE ( 'NONE', 'NONE',  #27915 ) ;
#5559 = CARTESIAN_POINT ( 'NONE',  ( 0.3976891862754212137, 0.7181140751201200434, -0.6642661073933326943 ) ) ;
#5560 = VERTEX_POINT ( 'NONE', #16357 ) ;
#5561 = CIRCLE ( 'NONE', #21360, 0.5905511811023621549 ) ;
#5562 = CARTESIAN_POINT ( 'NONE',  ( -0.04632226222404308563, 0.3520598332080951964, 1.953740157480315043 ) ) ;
#5563 = ORIENTED_EDGE ( 'NONE', *, *, #26212, .T. ) ;
#5564 = B_SPLINE_CURVE_WITH_KNOTS ( 'NONE', 3,
 ( #9552, #11972, #5332, #24395 ),
 .UNSPECIFIED., .F., .F.,
 ( 4, 4 ),
 ( 0.000000000000000000, 1.000000000000000000 ),
 .UNSPECIFIED. ) ;
#5565 = CARTESIAN_POINT ( 'NONE',  ( 0.5869493968219645641, -0.4267795243146149664, 5.226543307086613929E-17 ) ) ;
#5566 = CARTESIAN_POINT ( 'NONE',  ( -0.02559055118110236185, 0.000000000000000000, 0.000000000000000000 ) ) ;
#5567 = DIRECTION ( 'NONE',  ( -1.000000000000000000, 0.000000000000000000, 0.000000000000000000 ) ) ;
#5568 = CARTESIAN_POINT ( 'NONE',  ( -0.7874015748031496509, 0.3943205132762559462, -0.07664873632799094894 ) ) ;
#5569 = CARTESIAN_POINT ( 'NONE',  ( 0.07874015748031495954, 0.1968503937007874127, -3.364501312335958172 ) ) ;
#5570 = CARTESIAN_POINT ( 'NONE',  ( 0.1707210962531913734, -0.4707890492249701131, 0.2574803149606298969 ) ) ;
#5571 = ORIENTED_EDGE ( 'NONE', *, *, #25191, .T. ) ;
#5572 = EDGE_CURVE ( 'NONE', #24310, #21309, #423, .T. ) ;
#5573 = FACE_OUTER_BOUND ( 'NONE', #14108, .T. ) ;
#5574 = CIRCLE ( 'NONE', #8280, 0.1299232283464567539 ) ;
#5575 = CARTESIAN_POINT ( 'NONE',  ( -0.07874015748031495954, 0.000000000000000000, 0.4330708661417322913 ) ) ;
#5576 = AXIS2_PLACEMENT_3D ( 'NONE', #16947, #3950, #3358 ) ;
#5577 = CARTESIAN_POINT ( 'NONE',  ( 0.3460530745557667820, -0.09275304139126368252, -3.115157480314960647 ) ) ;
#5578 = ORIENTED_EDGE ( 'NONE', *, *, #25900, .T. ) ;
#5579 = CARTESIAN_POINT ( 'NONE',  ( 0.1152775731716972618, -0.4303822302053990634, -1.934055118110236338 ) ) ;
#5580 = AXIS2_PLACEMENT_3D ( 'NONE', #26578, #23829, #22353 ) ;
#5581 = ADVANCED_FACE ( 'NONE', ( #7596, #8537 ), #20447, .T. ) ;
#5582 = ORIENTED_EDGE ( 'NONE', *, *, #57, .F. ) ;
#5583 = CARTESIAN_POINT ( 'NONE',  ( 0.07874015748031495954, 0.1968503937007873850, -3.548228346456692162 ) ) ;
#5584 = DIRECTION ( 'NONE',  ( 0.000000000000000000, 0.000000000000000000, -1.000000000000000000 ) ) ;
#5585 = CARTESIAN_POINT ( 'NONE',  ( -0.4612490782034865955, 0.2663596103035612561, 1.747047244094488194 ) ) ;
#5586 = ADVANCED_FACE ( 'NONE', ( #18590 ), #13959, .T. ) ;
#5587 = EDGE_LOOP ( 'NONE', ( #13267, #5293 ) ) ;
#5588 = VERTEX_POINT ( 'NONE', #22708 ) ;
#5589 = LINE ( 'NONE', #3442, #7088 ) ;
#5590 = CONICAL_SURFACE ( 'NONE', #13249, 0.2952755905264887182, 0.2617993876495733341 ) ;
#5591 = CARTESIAN_POINT ( 'NONE',  ( -0.3644697409450258219, -0.09762295995070061072, -3.100567304031765836 ) ) ;
#5592 = CIRCLE ( 'NONE', #14654, 0.7165354330708662012 ) ;
#5593 = CARTESIAN_POINT ( 'NONE',  ( 1.197070535079588716, 0.07874015748031491790, 1.315180771300060503 ) ) ;
#5594 = LINE ( 'NONE', #1222, #6450 ) ;
#5595 = ORIENTED_EDGE ( 'NONE', *, *, #8491, .F. ) ;
#5596 = DIRECTION ( 'NONE',  ( -1.000000000000000000, 0.000000000000000000, 0.000000000000000000 ) ) ;
#5597 = PLANE ( 'NONE',  #8701 ) ;
#5598 = CARTESIAN_POINT ( 'NONE',  ( 0.0006679551606482677165, 0.5322830454629158270, 0.3401574803149606252 ) ) ;
#5599 = VERTEX_POINT ( 'NONE', #1245 ) ;
#5600 = CARTESIAN_POINT ( 'NONE',  ( 0.2712027394948776093, -0.3535065162672919037, -1.934055118110236338 ) ) ;
#5601 = EDGE_LOOP ( 'NONE', ( #11782, #25405, #3477, #10617 ) ) ;
#5602 = VERTEX_POINT ( 'NONE', #3334 ) ;
#5603 = CARTESIAN_POINT ( 'NONE',  ( -0.2131049448083992270, -0.5835666837866889667, 0.09685039370078740717 ) ) ;
#5604 = DIRECTION ( 'NONE',  ( 0.000000000000000000, 0.000000000000000000, 1.000000000000000000 ) ) ;
#5605 = CIRCLE ( 'NONE', #7384, 0.4807043897637795493 ) ;
#5606 = ADVANCED_FACE ( 'NONE', ( #27374 ), #4160, .T. ) ;
#5607 = CARTESIAN_POINT ( 'NONE',  ( 0.2362439534887394721, -0.2693339498142455213, -3.115157480314960647 ) ) ;
#5608 = CARTESIAN_POINT ( 'NONE',  ( 0.000000000000000000, 0.000000000000000000, 0.4724409448818898127 ) ) ;
#5609 = CARTESIAN_POINT ( 'NONE',  ( 0.3070866141732283561, 0.000000000000000000, 0.01181102362204724393 ) ) ;
#5610 = CARTESIAN_POINT ( 'NONE',  ( -0.3334645669291338987, 1.279353152430305007, -0.8465078874097147210 ) ) ;
#5611 = DIRECTION ( 'NONE',  ( 0.000000000000000000, 0.000000000000000000, 1.000000000000000000 ) ) ;
#5612 = CIRCLE ( 'NONE', #14189, 0.07910393700787400617 ) ;
#5613 = CARTESIAN_POINT ( 'NONE',  ( 0.04380501567505449417, -0.3346456692913384878, 1.973425196850393970 ) ) ;
#5614 = CONICAL_SURFACE ( 'NONE', #21405, 0.5511811023268710086, 0.7853981642949031672 ) ;
#5615 = ORIENTED_EDGE ( 'NONE', *, *, #7592, .T. ) ;
#5616 = CARTESIAN_POINT ( 'NONE',  ( -0.03937007874015747977, 0.8267716535433071723, 0.000000000000000000 ) ) ;
#5617 = EDGE_CURVE ( 'NONE', #9929, #1699, #22039, .T. ) ;
#5618 = DIRECTION ( 'NONE',  ( 0.000000000000000000, -1.000000000000000000, 0.000000000000000000 ) ) ;
#5619 = ORIENTED_EDGE ( 'NONE', *, *, #12525, .T. ) ;
#5620 = EDGE_LOOP ( 'NONE', ( #20522, #13116, #10840, #13234 ) ) ;
#5621 = LINE ( 'NONE', #21395, #16197 ) ;
#5622 = DIRECTION ( 'NONE',  ( -0.2225209339563147537, -0.9749279121818235083, 0.000000000000000000 ) ) ;
#5623 = CARTESIAN_POINT ( 'NONE',  ( -0.4225965726692971769, 0.3242071728275127129, 1.747047244094488194 ) ) ;
#5624 = SHAPE_REPRESENTATION ( 'Tapered Roller Bearing 17x40x17', ( #11588 ), #3496 ) ;
#5625 = EDGE_CURVE ( 'NONE', #10367, #23405, #19331, .T. ) ;
#5626 = CARTESIAN_POINT ( 'NONE',  ( -0.06699507805369578350, -0.5085118447801426633, 1.766732283464566899 ) ) ;
#5627 = AXIS2_PLACEMENT_3D ( 'NONE', #7311, #11547, #26653 ) ;
#5628 = EDGE_CURVE ( 'NONE', #12967, #12297, #22501, .T. ) ;
#5629 = EDGE_LOOP ( 'NONE', ( #263, #5750, #23968, #18754, #6100, #16886, #18842, #7683, #18642, #4652, #14285, #12418, #11589, #13376 ) ) ;
#5630 = CARTESIAN_POINT ( 'NONE',  ( 0.000000000000000000, 0.000000000000000000, 0.2362204724409449064 ) ) ;
#5631 = ORIENTED_EDGE ( 'NONE', *, *, #14553, .T. ) ;
#5632 = CARTESIAN_POINT ( 'NONE',  ( -0.7874015748031496509, 0.4238173070432976197, -0.003642219101859566713 ) ) ;
#5633 = FACE_BOUND ( 'NONE', #5452, .T. ) ;
#5634 = ORIENTED_EDGE ( 'NONE', *, *, #18752, .T. ) ;
#5635 = VERTEX_POINT ( 'NONE', #7883 ) ;
#5636 = VECTOR ( 'NONE', #20203, 39.37007874015748143 ) ;
#5637 = CARTESIAN_POINT ( 'NONE',  ( -0.2466292688015002954, -0.4270824798167766612, -1.569881889763779625 ) ) ;
#5638 = LINE ( 'NONE', #22876, #7955 ) ;
#5639 = VECTOR ( 'NONE', #127, 39.37007874015748143 ) ;
#5640 = ORIENTED_EDGE ( 'NONE', *, *, #4237, .F. ) ;
#5641 = B_SPLINE_CURVE_WITH_KNOTS ( 'NONE', 3,
 ( #6324, #1796, #19023, #27658, #8307, #4063, #12668, #21296, #23567, #12807 ),
 .UNSPECIFIED., .F., .F.,
 ( 4, 2, 2, 2, 4 ),
 ( 0.000000000000000000, 0.2500000000000001665, 0.5000000000000001110, 0.7500000000000000000, 1.000000000000000000 ),
 .UNSPECIFIED. ) ;
#5642 = ORIENTED_EDGE ( 'NONE', *, *, #21640, .T. ) ;
#5643 = CONTEXT_DEPENDENT_SHAPE_REPRESENTATION ( #5304, #15475 ) ;
#5644 = CARTESIAN_POINT ( 'NONE',  ( 0.0004986409324224840142, 0.3484797321218875421, 0.1166443193928900224 ) ) ;
#5645 = CARTESIAN_POINT ( 'NONE',  ( -0.3661417322834645272, 0.9448818897637796255, -1.639108661417322569E-17 ) ) ;
#5646 = CARTESIAN_POINT ( 'NONE',  ( 0.8031496062992127261, 0.000000000000000000, -1.092739370078740131E-17 ) ) ;
#5647 = DIRECTION ( 'NONE',  ( 1.000000000000000000, 0.000000000000000000, 0.000000000000000000 ) ) ;
#5648 = CONICAL_SURFACE ( 'NONE', #25034, 0.08582677165393072516, 0.7853981625000011624 ) ;
#5649 = EDGE_CURVE ( 'NONE', #12934, #3201, #5621, .T. ) ;
#5650 = CARTESIAN_POINT ( 'NONE',  ( -0.3882259019046727655, 0.3087756353513817498, 0.2989974301419745517 ) ) ;
#5651 = UNCERTAINTY_MEASURE_WITH_UNIT (LENGTH_MEASURE( 1.000000000000000082E-05 ), #224, 'distance_accuracy_value', 'NONE') ;
#5652 = EDGE_LOOP ( 'NONE', ( #9370, #6715, #3313, #11492, #23116, #3279 ) ) ;
#5653 = DIRECTION ( 'NONE',  ( 0.000000000000000000, 0.000000000000000000, 1.000000000000000000 ) ) ;
#5654 = FACE_OUTER_BOUND ( 'NONE', #7739, .T. ) ;
#5655 = DIRECTION ( 'NONE',  ( 0.7071067811865470176, 0.7071067811865480168, 0.000000000000000000 ) ) ;
#5656 = B_SPLINE_CURVE_WITH_KNOTS ( 'NONE', 2,
 ( #15649, #2499, #26097 ),
 .UNSPECIFIED., .F., .F.,
 ( 3, 3 ),
 ( 0.000000000000000000, 1.000000000000000000 ),
 .UNSPECIFIED. ) ;
#5657 = CARTESIAN_POINT ( 'NONE',  ( -0.5945615373477443066, -0.2192526351142929930, 0.2174344697355220513 ) ) ;
#5658 = AXIS2_PLACEMENT_3D ( 'NONE', #16841, #14751, #17254 ) ;
#5659 = CARTESIAN_POINT ( 'NONE',  ( -0.2420394123212937232, 0.2892587550802429575, 0.07637795275590551769 ) ) ;
#5660 = CYLINDRICAL_SURFACE ( 'NONE', #11486, 0.2952755905511805778 ) ;
#5661 = ORIENTED_EDGE ( 'NONE', *, *, #13984, .T. ) ;
#5662 = CARTESIAN_POINT ( 'NONE',  ( 0.3056525133779917636, 0.3651631491557606468, 0.1212655228624319320 ) ) ;
#5663 = ORIENTED_EDGE ( 'NONE', *, *, #19218, .T. ) ;
#5664 = ( NAMED_UNIT ( * ) SI_UNIT ( $, .STERADIAN. ) SOLID_ANGLE_UNIT ( ) ) ;
#5665 = CIRCLE ( 'NONE', #24152, 0.1771653543307086520 ) ;
#5666 = EDGE_LOOP ( 'NONE', ( #4615, #16993 ) ) ;
#5667 = B_SPLINE_CURVE_WITH_KNOTS ( 'NONE', 3,
 ( #26188, #17698, #21960, #22085, #4845, #21685 ),
 .UNSPECIFIED., .F., .F.,
 ( 4, 2, 4 ),
 ( 0.000000000000000000, 0.2500000000000000000, 0.5000000000000000000 ),
 .UNSPECIFIED. ) ;
#5668 = CYLINDRICAL_SURFACE ( 'NONE', #16513, 0.5118110236220472231 ) ;
#5669 = DIRECTION ( 'NONE',  ( 0.000000000000000000, 0.000000000000000000, -1.000000000000000000 ) ) ;
#5670 = CARTESIAN_POINT ( 'NONE',  ( 0.08600259748440709784, 0.2165354330708661457, -3.597797143241304951 ) ) ;
#5671 = ORIENTED_EDGE ( 'NONE', *, *, #9315, .F. ) ;
#5672 = CARTESIAN_POINT ( 'NONE',  ( -0.2988215684304370012, -0.6199272547993012195, 0.3401599409343967761 ) ) ;
#5673 = VERTEX_POINT ( 'NONE', #26183 ) ;
#5674 = AXIS2_PLACEMENT_3D ( 'NONE', #2622, #7149, #279 ) ;
#5675 = FILL_AREA_STYLE ('',( #23053 ) ) ;
#5676 = AXIS2_PLACEMENT_3D ( 'NONE', #21516, #25751, #21784 ) ;
#5677 = CARTESIAN_POINT ( 'NONE',  ( -0.0005963271530349164564, 0.4972008316437025455, 0.1140743250946061466 ) ) ;
#5678 = CARTESIAN_POINT ( 'NONE',  ( -0.2315507648392299000, -0.4792806379917101678, 0.3401574803149606252 ) ) ;
#5679 = EDGE_CURVE ( 'NONE', #21273, #23783, #24290, .T. ) ;
#5680 = EDGE_CURVE ( 'NONE', #22837, #17502, #17087, .T. ) ;
#5681 = ADVANCED_FACE ( 'NONE', ( #9205, #15464 ), #4700, .T. ) ;
#5682 = AXIS2_PLACEMENT_3D ( 'NONE', #7150, #15772, #26924 ) ;
#5683 = CARTESIAN_POINT ( 'NONE',  ( 0.003937007874015826907, -4.406857903543305967E-18, -0.09842519685039370636 ) ) ;
#5684 = CARTESIAN_POINT ( 'NONE',  ( -0.6119360453657027854, 0.1072290460172413279, 0.2574803149606298969 ) ) ;
#5685 = PRODUCT_RELATED_PRODUCT_CATEGORY ( 'part', '', ( #5510 ) ) ;
#5686 = ORIENTED_EDGE ( 'NONE', *, *, #348, .T. ) ;
#5687 = CARTESIAN_POINT ( 'NONE',  ( 0.3382184156749452608, -0.3855916753034395184, -1.550196850393700920 ) ) ;
#5688 = EDGE_CURVE ( 'NONE', #27195, #3027, #10932, .T. ) ;
#5689 = AXIS2_PLACEMENT_3D ( 'NONE', #21404, #8545, #17163 ) ;
#5690 = CARTESIAN_POINT ( 'NONE',  ( 0.3387265385688508212, 0.4407612517155324316, 0.9202755905511812440 ) ) ;
#5691 = CARTESIAN_POINT ( 'NONE',  ( -0.5511811023622048555, 0.000000000000000000, 0.9399606299212598381 ) ) ;
#5692 = CARTESIAN_POINT ( 'NONE',  ( -0.3105951325233360372, -0.1787383246550589000, 0.1805249803389203656 ) ) ;
#5693 = EDGE_CURVE ( 'NONE', #1064, #23265, #21674, .T. ) ;
#5694 = EDGE_CURVE ( 'NONE', #17378, #25403, #4836, .T. ) ;
#5695 = CARTESIAN_POINT ( 'NONE',  ( 0.5869493968219645641, 0.2133897621573074832, 0.3696019098714952711 ) ) ;
#5696 = VERTEX_POINT ( 'NONE', #2178 ) ;
#5697 = CARTESIAN_POINT ( 'NONE',  ( -0.2952755905264887182, 3.616083068046089993E-17, 0.9055118110027171596 ) ) ;
#5698 = ( NAMED_UNIT ( * ) SI_UNIT ( $, .STERADIAN. ) SOLID_ANGLE_UNIT ( ) ) ;
#5699 = CIRCLE ( 'NONE', #20574, 0.6212598425196850238 ) ;
#5700 = CARTESIAN_POINT ( 'NONE',  ( 0.4895462770359960136, 0.6604130065487362478, -0.5726600247964968027 ) ) ;
#5701 = CARTESIAN_POINT ( 'NONE',  ( -0.3511586785142654654, 0.4004922687717341612, 1.747047244094488194 ) ) ;
#5702 = VERTEX_POINT ( 'NONE', #15054 ) ;
#5703 = CIRCLE ( 'NONE', #21040, 0.4606299212598425341 ) ;
#5704 = EDGE_LOOP ( 'NONE', ( #1264, #5640, #5203, #4178 ) ) ;
#5705 = DIRECTION ( 'NONE',  ( 0.000000000000000000, 0.000000000000000000, 1.000000000000000000 ) ) ;
#5706 = CARTESIAN_POINT ( 'NONE',  ( -0.7165354330708662012, 8.847349907225958695E-17, 0.3543307086614173040 ) ) ;
#5707 = ORIENTED_EDGE ( 'NONE', *, *, #22683, .F. ) ;
#5708 = CARTESIAN_POINT ( 'NONE',  ( -0.1247869790646078808, -0.3443449117933338188, 0.1910323753003610736 ) ) ;
#5709 = CARTESIAN_POINT ( 'NONE',  ( -3.616083068348483797E-17, -0.2952755905511810774, 0.1377952755905511861 ) ) ;
#5710 = ORIENTED_EDGE ( 'NONE', *, *, #17648, .F. ) ;
#5711 = ORIENTED_EDGE ( 'NONE', *, *, #9036, .F. ) ;
#5712 = DIRECTION ( 'NONE',  ( -1.000000000000000000, 0.000000000000000000, 0.000000000000000000 ) ) ;
#5713 = DIRECTION ( 'NONE',  ( -1.000000000000000000, 0.000000000000000000, 0.000000000000000000 ) ) ;
#5714 = CARTESIAN_POINT ( 'NONE',  ( -0.09333834261715735769, 0.3008238710200430988, -3.240734708634343875 ) ) ;
#5715 = DIRECTION ( 'NONE',  ( -0.9930684569549264040, -0.1175373974578370340, 1.439418000000000363E-17 ) ) ;
#5716 = CARTESIAN_POINT ( 'NONE',  ( 0.6882266799383700562, -0.3690762517716402180, 0.03266564387697358518 ) ) ;
#5717 = VERTEX_POINT ( 'NONE', #23668 ) ;
#5718 = CARTESIAN_POINT ( 'NONE',  ( -0.2122766679520082800, -0.5838685267775929333, 0.2574827755769819038 ) ) ;
#5719 = CARTESIAN_POINT ( 'NONE',  ( -0.09842519685039370636, 0.07874015748031495954, -0.04546065111729338803 ) ) ;
#5720 = LINE ( 'NONE', #2322, #1854 ) ;
#5721 = CARTESIAN_POINT ( 'NONE',  ( 0.4921259842519685179, 0.5905511811023621549, 0.000000000000000000 ) ) ;
#5722 = TOROIDAL_SURFACE ( 'NONE', #9773, 0.5610236220472440971, 0.1003937007874015908 ) ;
#5723 = ADVANCED_FACE ( 'NONE', ( #3687 ), #27495, .F. ) ;
#5724 = CARTESIAN_POINT ( 'NONE',  ( -0.3213059197594588245, -0.1584813376851955946, -3.115157480314960647 ) ) ;
#5725 = ADVANCED_FACE ( 'NONE', ( #16848 ), #5223, .T. ) ;
#5726 = PRODUCT_DEFINITION_CONTEXT ( 'detailed design', #25319, 'design' ) ;
#5727 = ORIENTED_EDGE ( 'NONE', *, *, #19126, .F. ) ;
#5728 = CARTESIAN_POINT ( 'NONE',  ( 0.2712027394948692827, 0.3535065162672724748, -1.934055118110236338 ) ) ;
#5729 = AXIS2_PLACEMENT_3D ( 'NONE', #9022, #19640, #24147 ) ;
#5730 = EDGE_CURVE ( 'NONE', #11103, #9119, #22977, .T. ) ;
#5731 = ORIENTED_EDGE ( 'NONE', *, *, #16111, .F. ) ;
#5732 = ORIENTED_EDGE ( 'NONE', *, *, #4509, .T. ) ;
#5733 = CARTESIAN_POINT ( 'NONE',  ( 0.09842519685039370636, 0.2165354330708661457, -3.548228346456692162 ) ) ;
#5734 = DIRECTION ( 'NONE',  ( 1.000000000000000000, 0.000000000000000000, 0.000000000000000000 ) ) ;
#5735 = CARTESIAN_POINT ( 'NONE',  ( -0.4004221243553298115, -0.3512268162760094348, 1.747047244094488194 ) ) ;
#5736 = ORIENTED_EDGE ( 'NONE', *, *, #26852, .F. ) ;
#5737 = DIRECTION ( 'NONE',  ( 0.000000000000000000, 1.000000000000000000, 0.000000000000000000 ) ) ;
#5738 = ADVANCED_FACE ( 'NONE', ( #8467 ), #22051, .F. ) ;
#5739 = EDGE_LOOP ( 'NONE', ( #21715, #3961, #23435, #27138 ) ) ;
#5740 = CARTESIAN_POINT ( 'NONE',  ( -0.1213180142433854664, 0.3572819248074437515, -3.100567304031767168 ) ) ;
#5741 = AXIS2_PLACEMENT_3D ( 'NONE', #23293, #5377, #18201 ) ;
#5742 = CARTESIAN_POINT ( 'NONE',  ( 0.2146455952141596568, -0.4472013107316724079, 0.1734435147974487113 ) ) ;
#5743 = B_SPLINE_SURFACE_WITH_KNOTS ( 'NONE', 2, 3, ( 
 ( #5346, #18605, #20461, #14107, #25685, #27531, #3788, #12955, #12407, #14556, #27810, #8175, #4214, #19318, #8444, #10702, #14834, #10416, #12549, #16788, #17204, #19179, #12679, #18889, #25401, #8041, #6065, #4075, #23714, #21022, #16935, #23154, #21308, #23445, #4350, #21451, #1668, #25258, #12819, #6470, #14697, #2090, #23304, #3932, #25545, #1808, #1945, #18753, #15105, #10276, #10556, #21166, #1529, #19034, #8586, #17067, #10137, #27669, #23580, #8317, #6336, #6205, #5921, #21, #14966, #25823 ),
 ( #27388, #16649, #2495, #26357, #2351, #8722, #26487, #8854, #283, #15513, #19873, #9117, #13498, #5020, #7021, #17865, #11116, #21584, #4887, #10843, #17736, #6753, #22125, #15644, #19608, #23852, #19457, #4490, #6612, #526, #26094, #24243, #11387, #2755, #20005, #6884, #19736, #13233, #15386, #9244, #11252, #4745, #10982, #23973, #17344, #21857, #24112, #13097, #405, #8988, #25960, #17612, #26226, #21993, #656, #2626, #7153, #15775, #15238, #24377, #21722, #26774, #7422, #27070, #26629, #14223 ),
 ( #23406, #27349, #1768, #4040, #10734, #18847, #21127, #27773, #6021, #14657, #14513, #20983, #5745, #12511, #1490, #12646, #4177, #17035, #17169, #25508, #8550, #23543, #14360, #10102, #25214, #21410, #5886, #3890, #21274, #8000, #10380, #1909, #22974, #27490, #19000, #8413, #23261, #27633, #23115, #1629, #3596, #8278, #18713, #10520, #12782, #25646, #12225, #20840, #3744, #16898, #16603, #14800, #19140, #12365, #6300, #10234, #8138, #14934, #19283, #16747, #2048, #25359, #13064, #13193, #26058, #8952 ) ),
 .UNSPECIFIED., .F., .T., .F.,
 ( 3, 3 ),
 ( 4, 2, 2, 2, 2, 2, 2, 2, 2, 2, 2, 2, 2, 2, 2, 2, 2, 2, 2, 2, 2, 2, 2, 2, 2, 2, 2, 2, 2, 2, 2, 2, 4 ),
 ( 0.000000000000000000, 1.000000000000000000 ),
 ( 0.000000000000000000, 0.1963495408493620697, 0.3926990816987241395, 0.5890486225480862092, 0.7853981633974482790, 0.9817477042468103487, 1.178097245096172418, 1.374446785945534488, 1.570796326794896558, 1.767145867644258628, 1.963495408493620697, 2.159844949342982545, 2.356194490192344837, 2.552544031041707129, 2.748893571891068976, 2.945243112740430824, 3.141592653589793116, 3.337942194439155408, 3.534291735288517255, 3.730641276137879103, 3.926990816987241395, 4.123340357836603687, 4.319689898685965090, 4.516039439535327382, 4.712388980384689674, 4.908738521234051966, 5.105088062083414258, 5.301437602932775661, 5.497787143782137953, 5.694136684631500245, 5.890486225480861648, 6.086835766330223940, 6.283185307179586232 ),
 .UNSPECIFIED. ) ;
#5744 = DIRECTION ( 'NONE',  ( 1.000000000000000000, 0.000000000000000000, 0.000000000000000000 ) ) ;
#5745 = CARTESIAN_POINT ( 'NONE',  ( 0.1570220809524471017, 0.3184841198566427112, 1.953740157480315043 ) ) ;
#5746 = ORIENTED_EDGE ( 'NONE', *, *, #16205, .T. ) ;
#5747 = CARTESIAN_POINT ( 'NONE',  ( -0.4032359719620975946, -0.5930303427490664081, -0.4910027445640789412 ) ) ;
#5749 = CARTESIAN_POINT ( 'NONE',  ( -0.1480156394741914683, 0.5526079293737398146, 0.9399606299212598381 ) ) ;
#5748 = CARTESIAN_POINT ( 'NONE',  ( -1.197070535079588716, 0.07874015748031495954, -1.197070535079588716 ) ) ;
#5750 = ORIENTED_EDGE ( 'NONE', *, *, #12274, .T. ) ;
#5751 = DIRECTION ( 'NONE',  ( 0.000000000000000000, -1.000000000000000000, 0.000000000000000000 ) ) ;
#5752 = ORIENTED_EDGE ( 'NONE', *, *, #10357, .F. ) ;
#5753 = CARTESIAN_POINT ( 'NONE',  ( 0.0004974201395668471654, 0.3464563358313494934, 0.1377952755905513249 ) ) ;
#5754 = DIRECTION ( 'NONE',  ( -1.000000000000000000, 0.000000000000000000, 0.000000000000000000 ) ) ;
#5755 = CARTESIAN_POINT ( 'NONE',  ( -0.3102476824511484210, -0.1791601451668926870, -3.115157480314960647 ) ) ;
#5756 = CARTESIAN_POINT ( 'NONE',  ( 0.000000000000000000, 0.4724409448818898127, -1.811023622047243542 ) ) ;
#5757 = CARTESIAN_POINT ( 'NONE',  ( -0.6299212598425196763, 0.9448818897637796255, -9.561468503937007847E-18 ) ) ;
#5758 = CARTESIAN_POINT ( 'NONE',  ( -0.3334645669291338987, 1.123031841058557134, -0.8716920363354115908 ) ) ;
#5759 = EDGE_CURVE ( 'NONE', #26083, #24281, #23468, .T. ) ;
#5760 = ( BOUNDED_CURVE ( )  B_SPLINE_CURVE ( 2, ( #5803, #3656, #1689 ),
 .UNSPECIFIED., .F., .T. ) 
 B_SPLINE_CURVE_WITH_KNOTS ( ( 3, 3 ),
 ( 0.000000000000000000, 0.5842180690389568998 ),
 .UNSPECIFIED. ) 
 CURVE ( )  GEOMETRIC_REPRESENTATION_ITEM ( )  RATIONAL_B_SPLINE_CURVE ( ( 1.000000000000000000, 1.154700538379249908, 1.000000000000000000 ) ) 
 REPRESENTATION_ITEM ( '' )  ) ;
#5761 = DIRECTION ( 'NONE',  ( 1.000000000000000000, 0.000000000000000000, 0.000000000000000000 ) ) ;
#5762 = DIRECTION ( 'NONE',  ( 0.000000000000000000, 0.000000000000000000, -1.000000000000000000 ) ) ;
#5763 = CARTESIAN_POINT ( 'NONE',  ( 0.5376957092749897749, -0.3112026930391976753, 0.2574803149606298969 ) ) ;
#5764 = CIRCLE ( 'NONE', #27414, 0.4941010236220472751 ) ;
#5765 = EDGE_LOOP ( 'NONE', ( #6628, #2502, #24974, #21666, #6750, #20699 ) ) ;
#5766 = LINE ( 'NONE', #6191, #9622 ) ;
#5767 = CARTESIAN_POINT ( 'NONE',  ( 0.000000000000000000, 0.000000000000000000, -4.330708661417323135 ) ) ;
#5768 = CARTESIAN_POINT ( 'NONE',  ( 0.000000000000000000, 0.000000000000000000, 0.01181102362204724393 ) ) ;
#5769 = VERTEX_POINT ( 'NONE', #2112 ) ;
#5770 = DIRECTION ( 'NONE',  ( 0.000000000000000000, 0.000000000000000000, -1.000000000000000000 ) ) ;
#5771 = CARTESIAN_POINT ( 'NONE',  ( 0.4055118110236220486, 0.000000000000000000, -1.639108858267716421E-17 ) ) ;
#5772 = CARTESIAN_POINT ( 'NONE',  ( 0.000000000000000000, 0.000000000000000000, 0.1992125984251968684 ) ) ;
#5773 = CARTESIAN_POINT ( 'NONE',  ( -0.4856708409200654608, 0.1649135259617025839, 1.766732283464566899 ) ) ;
#5774 = ORIENTED_EDGE ( 'NONE', *, *, #27188, .T. ) ;
#5775 = ORIENTED_EDGE ( 'NONE', *, *, #13391, .F. ) ;
#5776 = CARTESIAN_POINT ( 'NONE',  ( -0.1968503937007874127, 1.092519685039370136, 1.362057955722570717E-16 ) ) ;
#5777 = ORIENTED_EDGE ( 'NONE', *, *, #3202, .F. ) ;
#5778 = CARTESIAN_POINT ( 'NONE',  ( -0.7874015748031496509, 0.4533141008103401259, 0.06936429812427165331 ) ) ;
#5779 = LENGTH_MEASURE_WITH_UNIT ( LENGTH_MEASURE( 0.02539999999999999897 ), #11694 ) ;
#5780 = DIRECTION ( 'NONE',  ( 0.000000000000000000, 0.000000000000000000, 1.000000000000000000 ) ) ;
#5781 = AXIS2_PLACEMENT_3D ( 'NONE', #3111, #9903, #22483 ) ;
#5782 = CARTESIAN_POINT ( 'NONE',  ( 3.168943700787402105E-16, -0.6299212598425196763, 0.000000000000000000 ) ) ;
#5783 = ORIENTED_EDGE ( 'NONE', *, *, #7586, .F. ) ;
#5784 = VERTEX_POINT ( 'NONE', #18914 ) ;
#5785 = CARTESIAN_POINT ( 'NONE',  ( 0.03220957031753916844, -0.4921259842519685179, -1.550196850393700920 ) ) ;
#5786 = PRODUCT_DEFINITION_FORMATION_WITH_SPECIFIED_SOURCE ( 'ANY', '', #10231, .NOT_KNOWN. ) ;
#5787 = ORIENTED_EDGE ( 'NONE', *, *, #7947, .F. ) ;
#5788 = ORIENTED_EDGE ( 'NONE', *, *, #19691, .T. ) ;
#5789 = ORIENTED_EDGE ( 'NONE', *, *, #6150, .F. ) ;
#5790 = AXIS2_PLACEMENT_3D ( 'NONE', #17138, #21937, #11057 ) ;
#5791 = DIRECTION ( 'NONE',  ( 0.000000000000000000, 0.000000000000000000, 1.000000000000000000 ) ) ;
#5792 = DIRECTION ( 'NONE',  ( 0.2384530002628495460, 2.920207035189816837E-17, -0.9711540385879292581 ) ) ;
#5793 = CARTESIAN_POINT ( 'NONE',  ( 0.000000000000000000, 0.000000000000000000, 0.2755905511811023723 ) ) ;
#5794 = EDGE_CURVE ( 'NONE', #26373, #18491, #17329, .T. ) ;
#5795 = VERTEX_POINT ( 'NONE', #17226 ) ;
#5796 = DIRECTION ( 'NONE',  ( 1.000000000000000000, 0.000000000000000000, 0.000000000000000000 ) ) ;
#5797 = CIRCLE ( 'NONE', #4862, 0.5007874015748031704 ) ;
#5798 = DIRECTION ( 'NONE',  ( 0.7071067818211390632, -8.659560554583428975E-17, -0.7071067805519560823 ) ) ;
#5799 = DIRECTION ( 'NONE',  ( 0.000000000000000000, -0.7071067818211396183, -0.7071067805519553051 ) ) ;
#5800 = DIRECTION ( 'NONE',  ( -1.000000000000000000, -1.000000000000000078E-15, 0.000000000000000000 ) ) ;
#5801 = CARTESIAN_POINT ( 'NONE',  ( -0.5642276165568446133, -0.3262508299432601011, 0.1942441824117969729 ) ) ;
#5802 = AXIS2_PLACEMENT_3D ( 'NONE', #4047, #1500, #12653 ) ;
#5803 = CARTESIAN_POINT ( 'NONE',  ( 0.03008364706454716778, -0.1136516277932324709, -0.1968503937007874127 ) ) ;
#5804 = AXIS2_PLACEMENT_3D ( 'NONE', #12901, #11063, #19813 ) ;
#5805 = CYLINDRICAL_SURFACE ( 'NONE', #2443, 0.09842519685039370636 ) ;
#5806 = FACE_OUTER_BOUND ( 'NONE', #5458, .T. ) ;
#5807 = ORIENTED_EDGE ( 'NONE', *, *, #26124, .F. ) ;
#5808 = ORIENTED_EDGE ( 'NONE', *, *, #17183, .T. ) ;
#5809 = DIRECTION ( 'NONE',  ( -1.000000000000000000, -1.224646799147356165E-16, 0.000000000000000000 ) ) ;
#5810 = ORIENTED_EDGE ( 'NONE', *, *, #6051, .T. ) ;
#5811 = CARTESIAN_POINT ( 'NONE',  ( -0.09842519685039370636, 2.800920866141732248E-17, 0.09092130223458683158 ) ) ;
#5812 = LINE ( 'NONE', #14291, #15302 ) ;
#5813 = DIMENSIONAL_EXPONENTS ( 1.000000000000000000, 0.000000000000000000, 0.000000000000000000, 0.000000000000000000, 0.000000000000000000, 0.000000000000000000, 0.000000000000000000 ) ;
#5814 = ORIENTED_EDGE ( 'NONE', *, *, #13838, .F. ) ;
#5815 = DIRECTION ( 'NONE',  ( 1.224646799147353207E-16, 1.000000000000000000, -0.000000000000000000 ) ) ;
#5816 = VERTEX_POINT ( 'NONE', #6637 ) ;
#5817 = AXIS2_PLACEMENT_3D ( 'NONE', #2101, #10713, #12965 ) ;
#5818 = CARTESIAN_POINT ( 'NONE',  ( 0.1490609433615242285, 0.000000000000000000, 0.000000000000000000 ) ) ;
#5819 = AXIS2_PLACEMENT_3D ( 'NONE', #6562, #19553, #4443 ) ;
#5820 = CIRCLE ( 'NONE', #13027, 0.6299212598425196763 ) ;
#5821 = DIRECTION ( 'NONE',  ( -0.2036417511401769631, 0.9790454724845838452, 0.000000000000000000 ) ) ;
#5822 = CARTESIAN_POINT ( 'NONE',  ( 0.000000000000000000, 0.000000000000000000, 0.2574803149606298969 ) ) ;
#5823 = EDGE_CURVE ( 'NONE', #13865, #3709, #24715, .T. ) ;
#5824 = FACE_OUTER_BOUND ( 'NONE', #5620, .T. ) ;
#5825 = ORIENTED_EDGE ( 'NONE', *, *, #14340, .F. ) ;
#5826 = CARTESIAN_POINT ( 'NONE',  ( -0.2992781133269515892, -0.6197069291944330427, 0.1322834645669291320 ) ) ;
#5827 = VERTEX_POINT ( 'NONE', #1968 ) ;
#5828 = CIRCLE ( 'NONE', #11673, 0.5531496062992126150 ) ;
#5829 = VERTEX_POINT ( 'NONE', #10577 ) ;
#5830 = CARTESIAN_POINT ( 'NONE',  ( 0.02190250779246093876, -0.3346456692913385433, 1.973425196850393970 ) ) ;
#5831 = B_SPLINE_CURVE_WITH_KNOTS ( 'NONE', 3,
 ( #22998, #3617, #18303, #3192, #24817, #14090 ),
 .UNSPECIFIED., .F., .F.,
 ( 4, 2, 4 ),
 ( 0.3108507187342960387, 0.3125269569790670166, 0.3142031952238389936 ),
 .UNSPECIFIED. ) ;
#5832 = CARTESIAN_POINT ( 'NONE',  ( 0.2564944395535923571, -0.4441657790094409863, -1.550196850393700920 ) ) ;
#5833 = CARTESIAN_POINT ( 'NONE',  ( 0.000000000000000000, 0.000000000000000000, -0.1309055118110236116 ) ) ;
#5834 = CARTESIAN_POINT ( 'NONE',  ( 0.04448665381632212201, -0.06523692067838748887, -0.4653551329966303385 ) ) ;
#5835 = CARTESIAN_POINT ( 'NONE',  ( 0.3642352168757231889, -0.4152525734085952269, 0.9399606299212598381 ) ) ;
#5836 = CARTESIAN_POINT ( 'NONE',  ( -0.7874015748031496509, 0.000000000000000000, -1.052618110236220428 ) ) ;
#5837 = ORIENTED_EDGE ( 'NONE', *, *, #19961, .F. ) ;
#5838 = DIRECTION ( 'NONE',  ( 0.000000000000000000, 0.000000000000000000, -1.000000000000000000 ) ) ;
#5839 = AXIS2_PLACEMENT_3D ( 'NONE', #6183, #12928, #15212 ) ;
#5840 = CIRCLE ( 'NONE', #4908, 0.5007874015748031704 ) ;
#5841 = AXIS2_PLACEMENT_3D ( 'NONE', #9381, #11656, #26442 ) ;
#5842 = EDGE_LOOP ( 'NONE', ( #12784, #5438, #8571, #10405, #10856, #2127 ) ) ;
#5843 = ADVANCED_FACE ( 'NONE', ( #27830, #17088 ), #14986, .T. ) ;
#5844 = DIRECTION ( 'NONE',  ( 0.000000000000000000, 0.000000000000000000, 1.000000000000000000 ) ) ;
#5846 = CARTESIAN_POINT ( 'NONE',  ( 0.4130706566799093316, -0.6693539628600351232, 6.842164547144469713E-17 ) ) ;
#5845 = ( GEOMETRIC_REPRESENTATION_CONTEXT ( 3 ) GLOBAL_UNCERTAINTY_ASSIGNED_CONTEXT ( ( #9879 ) ) GLOBAL_UNIT_ASSIGNED_CONTEXT ( ( #9609, #3380, #14011 ) ) REPRESENTATION_CONTEXT ( 'NONE', 'WORKASPACE' ) ) ;
#5847 = CARTESIAN_POINT ( 'NONE',  ( 0.000000000000000000, 0.000000000000000000, -0.2342519685039370358 ) ) ;
#5848 = CARTESIAN_POINT ( 'NONE',  ( 0.5280876769849813801, -0.06947563356185804118, 1.747047244094488194 ) ) ;
#5849 = EDGE_LOOP ( 'NONE', ( #7073, #17608 ) ) ;
#5850 = CARTESIAN_POINT ( 'NONE',  ( -0.5670362563030384440, -0.5142385541158210893, 0.9905098495110491452 ) ) ;
#5851 = VERTEX_POINT ( 'NONE', #25843 ) ;
#5852 = FACE_OUTER_BOUND ( 'NONE', #21800, .T. ) ;
#5853 = CARTESIAN_POINT ( 'NONE',  ( 0.3105951325274823871, -0.1787383246574437701, 0.09506557083491969096 ) ) ;
#5854 = EDGE_CURVE ( 'NONE', #27249, #24718, #5883, .T. ) ;
#5855 = CARTESIAN_POINT ( 'NONE',  ( -0.0004974201395671521515, 0.3464563358313494934, 0.1377952755905512139 ) ) ;
#5856 = LINE ( 'NONE', #7831, #22622 ) ;
#5857 = CARTESIAN_POINT ( 'NONE',  ( 0.6882266799383700562, -0.4204501145275968965, 0.1837325802280523612 ) ) ;
#5858 = ORIENTED_EDGE ( 'NONE', *, *, #10075, .T. ) ;
#5859 = LENGTH_MEASURE_WITH_UNIT ( LENGTH_MEASURE( 0.02539999999999999897 ), #25193 ) ;
#5860 = CARTESIAN_POINT ( 'NONE',  ( -0.2938622683360632148, 3.727965067992227128E-17, -3.745078740157480546 ) ) ;
#5861 = AXIS2_PLACEMENT_3D ( 'NONE', #7438, #16067, #13946 ) ;
#5862 = DIRECTION ( 'NONE',  ( 0.000000000000000000, 0.000000000000000000, 1.000000000000000000 ) ) ;
#5863 = EDGE_LOOP ( 'NONE', ( #27588, #18953, #20127, #26995, #27493 ) ) ;
#5864 = CARTESIAN_POINT ( 'NONE',  ( 0.1584813376851776368, -0.3213059197594625993, -3.115157480314961980 ) ) ;
#5865 = ( REPRESENTATION_RELATIONSHIP ('NONE','NONE', #12434, #5415 ) REPRESENTATION_RELATIONSHIP_WITH_TRANSFORMATION ( #22589 )SHAPE_REPRESENTATION_RELATIONSHIP( ) ) ;
#5866 = CARTESIAN_POINT ( 'NONE',  ( 0.3001918266902144361, -0.3912931228432220410, -1.569881889763779625 ) ) ;
#5867 = ORIENTED_EDGE ( 'NONE', *, *, #7076, .T. ) ;
#5868 = CARTESIAN_POINT ( 'NONE',  ( -0.3858397471888894703, -0.2228126397719936702, -1.934055118110236338 ) ) ;
#5869 = ORIENTED_EDGE ( 'NONE', *, *, #27217, .T. ) ;
#5870 = ORIENTED_EDGE ( 'NONE', *, *, #1565, .T. ) ;
#5871 = ORIENTED_EDGE ( 'NONE', *, *, #7145, .T. ) ;
#5872 = ORIENTED_EDGE ( 'NONE', *, *, #25236, .T. ) ;
#5873 = CARTESIAN_POINT ( 'NONE',  ( -0.5743180011325290657, -0.2903071062613433173, 0.2032833715572389954 ) ) ;
#5874 = PRESENTATION_STYLE_ASSIGNMENT (( #23395 ) ) ;
#5875 = APPLICATION_PROTOCOL_DEFINITION ( 'draft international standard', 'automotive_design', 1998, #24776 ) ;
#5876 = CARTESIAN_POINT ( 'NONE',  ( 0.5085118447801502128, -0.06699507805371243685, 1.747047244094488194 ) ) ;
#5877 = ORIENTED_EDGE ( 'NONE', *, *, #25456, .F. ) ;
#5878 = EDGE_CURVE ( 'NONE', #5599, #22369, #23402, .T. ) ;
#5879 = AXIS2_PLACEMENT_3D ( 'NONE', #10428, #19043, #27677 ) ;
#5880 = CARTESIAN_POINT ( 'NONE',  ( 0.2296683860596781812, -0.2993674444872274631, -3.100567304031764060 ) ) ;
#5881 = EDGE_CURVE ( 'NONE', #2885, #8441, #18904, .T. ) ;
#5882 = CARTESIAN_POINT ( 'NONE',  ( 0.3013593406941685315, 0.3597456680659448791, 0.1992142434433716580 ) ) ;
#5883 = B_SPLINE_CURVE_WITH_KNOTS ( 'NONE', 3,
 ( #7270, #19990, #9234, #15889 ),
 .UNSPECIFIED., .F., .F.,
 ( 4, 4 ),
 ( 0.9359046326925629655, 0.9375808709372031036 ),
 .UNSPECIFIED. ) ;
#5884 = CARTESIAN_POINT ( 'NONE',  ( 0.1120675189988346587, -0.6505216398953739265, -0.1269869061606484217 ) ) ;
#5885 = EDGE_CURVE ( 'NONE', #16430, #4045, #24633, .T. ) ;
#5886 = CARTESIAN_POINT ( 'NONE',  ( -0.2817310484609166221, 0.2161381151963042424, 1.953740157480315043 ) ) ;
#5887 = VERTEX_POINT ( 'NONE', #25494 ) ;
#5888 = VERTEX_POINT ( 'NONE', #6836 ) ;
#5889 = CARTESIAN_POINT ( 'NONE',  ( -0.6128263037575037986, -0.09844888684487719532, -0.2421684138024215449 ) ) ;
#5890 = CARTESIAN_POINT ( 'NONE',  ( -0.1574803149606299191, -0.5905511811023621549, 7.232166136696967594E-17 ) ) ;
#5892 = CARTESIAN_POINT ( 'NONE',  ( 0.3482225189666449672, 0.4539000224941344697, 0.9399606299212598381 ) ) ;
#5891 = CARTESIAN_POINT ( 'NONE',  ( -0.3334645669291338987, 1.286842404713327115, -0.9809137335991812146 ) ) ;
#5893 = EDGE_CURVE ( 'NONE', #8859, #19876, #25740, .T. ) ;
#5894 = ORIENTED_EDGE ( 'NONE', *, *, #21466, .F. ) ;
#5895 = FACE_BOUND ( 'NONE', #4032, .T. ) ;
#5896 = DIRECTION ( 'NONE',  ( 0.000000000000000000, -1.000000000000000000, 0.000000000000000000 ) ) ;
#5897 = CARTESIAN_POINT ( 'NONE',  ( -0.09269288654274109029, 0.3460635936744927421, -3.115157480314960647 ) ) ;
#5898 = CARTESIAN_POINT ( 'NONE',  ( 0.000000000000000000, 0.8267716535433071723, 0.2362204724409449064 ) ) ;
#5899 = DIRECTION ( 'NONE',  ( 1.000000000000000000, 0.000000000000000000, 0.000000000000000000 ) ) ;
#5900 = CARTESIAN_POINT ( 'NONE',  ( 0.03532354024591720376, -0.07677165354330710290, 0.000000000000000000 ) ) ;
#5901 = DIRECTION ( 'NONE',  ( -1.000000000000000000, 0.000000000000000000, 0.000000000000000000 ) ) ;
#5902 = LINE ( 'NONE', #23280, #24082 ) ;
#5903 = CARTESIAN_POINT ( 'NONE',  ( 0.000000000000000000, 0.000000000000000000, 0.1771653543307086520 ) ) ;
#5904 = EDGE_LOOP ( 'NONE', ( #8750, #17527, #17002, #26771 ) ) ;
#5905 = CARTESIAN_POINT ( 'NONE',  ( -0.1481199686337219545, 0.5525886237725313732, 0.9399606299212598381 ) ) ;
#5906 = FACE_BOUND ( 'NONE', #26325, .T. ) ;
#5907 = EDGE_CURVE ( 'NONE', #25295, #23039, #2177, .T. ) ;
#5908 = CARTESIAN_POINT ( 'NONE',  ( 0.1755067523729419432, 0.6057501678605275997, 0.000000000000000000 ) ) ;
#5909 = FACE_OUTER_BOUND ( 'NONE', #24647, .T. ) ;
#5910 = LINE ( 'NONE', #12669, #19441 ) ;
#5911 = CARTESIAN_POINT ( 'NONE',  ( 0.1495939273659978308, -0.4806208190371700772, -0.02345246241341144428 ) ) ;
#5912 = CARTESIAN_POINT ( 'NONE',  ( 0.4069448477555986377, -0.3121994997598466770, 1.766732283464566899 ) ) ;
#5913 = VERTEX_POINT ( 'NONE', #4699 ) ;
#5914 = EDGE_CURVE ( 'NONE', #1942, #16391, #22730, .T. ) ;
#5915 = ORIENTED_EDGE ( 'NONE', *, *, #27409, .T. ) ;
#5916 = LINE ( 'NONE', #5490, #20087 ) ;
#5917 = VERTEX_POINT ( 'NONE', #13177 ) ;
#5918 = CARTESIAN_POINT ( 'NONE',  ( -0.4143937130580483963, 0.4928070724588058393, 0.1183902030367787600 ) ) ;
#5919 = PLANE ( 'NONE',  #564 ) ;
#5920 = EDGE_CURVE ( 'NONE', #23881, #15279, #6868, .T. ) ;
#5921 = CARTESIAN_POINT ( 'NONE',  ( 0.3239425792934409465, -0.08676778863010950471, 1.973425196850393970 ) ) ;
#5922 = VERTEX_POINT ( 'NONE', #1470 ) ;
#5923 = ORIENTED_EDGE ( 'NONE', *, *, #14871, .T. ) ;
#5924 = AXIS2_PLACEMENT_3D ( 'NONE', #24217, #4857, #916 ) ;
#5925 = CARTESIAN_POINT ( 'NONE',  ( -0.2180862235769588653, -0.4423390553432484107, -1.550196850393700920 ) ) ;
#5926 = DIRECTION ( 'NONE',  ( 0.000000000000000000, 0.000000000000000000, 1.000000000000000000 ) ) ;
#5927 = ORIENTED_EDGE ( 'NONE', *, *, #27300, .T. ) ;
#5928 = CIRCLE ( 'NONE', #22609, 0.3771653543307086909 ) ;
#5929 = B_SPLINE_CURVE_WITH_KNOTS ( 'NONE', 3,
 ( #13518, #4906, #21606, #17494, #15124, #13253, #15403, #2107, #22014, #4367, #25842 ),
 .UNSPECIFIED., .F., .F.,
 ( 4, 2, 1, 2, 2, 4 ),
 ( 0.5000000000000000000, 0.6250000000000006661, 0.6875000000000007772, 0.7187500000000007772, 0.7500000000000008882, 1.000000000000000000 ),
 .UNSPECIFIED. ) ;
#5930 = ITEM_DEFINED_TRANSFORMATION ( 'NONE', 'NONE', #24642,  #11588 ) ;
#5931 = DIRECTION ( 'NONE',  ( -1.000000000000000000, 0.000000000000000000, 0.000000000000000000 ) ) ;
#5932 = CARTESIAN_POINT ( 'NONE',  ( -0.2956505864974143805, 0.3532288989643738719, 0.1771653543307089018 ) ) ;
#5933 = DIRECTION ( 'NONE',  ( 0.000000000000000000, 1.000000000000000000, 0.000000000000000000 ) ) ;
#5934 = CARTESIAN_POINT ( 'NONE',  ( 0.03532354024591842501, -1.259842519685039353, 7.714310545810098438E-17 ) ) ;
#5935 = EDGE_CURVE ( 'NONE', #9678, #24096, #9875, .T. ) ;
#5936 = ORIENTED_EDGE ( 'NONE', *, *, #1219, .F. ) ;
#5937 = CARTESIAN_POINT ( 'NONE',  ( 0.09590060490395689585, 0.2273032555864669124, 0.000000000000000000 ) ) ;
#5938 = LINE ( 'NONE', #7912, #15070 ) ;
#5939 = FACE_BOUND ( 'NONE', #22118, .T. ) ;
#5940 = DIRECTION ( 'NONE',  ( -1.000000000000000078E-15, 1.000000000000000000, 0.000000000000000000 ) ) ;
#5941 = CIRCLE ( 'NONE', #27593, 0.5007874015748031704 ) ;
#5942 = CARTESIAN_POINT ( 'NONE',  ( -0.4958728716544008042, -0.5762407295275912000, 0.1026277124767580040 ) ) ;
#5943 = CARTESIAN_POINT ( 'NONE',  ( 0.000000000000000000, 0.000000000000000000, -4.330708661417323135 ) ) ;
#5944 = CARTESIAN_POINT ( 'NONE',  ( 0.000000000000000000, 0.000000000000000000, -0.07578740157480315376 ) ) ;
#5945 = CARTESIAN_POINT ( 'NONE',  ( -0.0006679551606482677165, 0.5322830454629158270, 0.1322834645669291320 ) ) ;
#5946 = DIRECTION ( 'NONE',  ( 0.000000000000000000, 0.000000000000000000, 1.000000000000000000 ) ) ;
#5947 = AXIS2_PLACEMENT_3D ( 'NONE', #19913, #11564, #22306 ) ;
#5948 = AXIS2_PLACEMENT_3D ( 'NONE', #14923, #25348, #18555 ) ;
#5950 = EDGE_CURVE ( 'NONE', #7273, #4205, #13910, .T. ) ;
#5949 = ORIENTED_EDGE ( 'NONE', *, *, #9973, .T. ) ;
#5951 = VERTEX_POINT ( 'NONE', #7549 ) ;
#5952 = EDGE_CURVE ( 'NONE', #19912, #830, #4822, .T. ) ;
#5953 = ORIENTED_EDGE ( 'NONE', *, *, #10677, .T. ) ;
#5954 = LINE ( 'NONE', #7786, #321 ) ;
#5955 = CARTESIAN_POINT ( 'NONE',  ( -0.3218523081051654078, -0.6665164569871881994, 0.2562996995972176006 ) ) ;
#5956 = CARTESIAN_POINT ( 'NONE',  ( -0.3642352168757148068, 0.4152525734086684461, 0.9202755905511811330 ) ) ;
#5957 = ORIENTED_EDGE ( 'NONE', *, *, #8181, .T. ) ;
#5958 = CARTESIAN_POINT ( 'NONE',  ( -0.2983664441502653641, -0.6201464311010354002, 0.3401599409343967761 ) ) ;
#5959 = B_SPLINE_CURVE_WITH_KNOTS ( 'NONE', 3,
 ( #11262, #22003, #948, #24119, #2763, #9538, #11395, #26495, #22268, #7161, #15913, #4755, #535, #9126, #18140, #26784, #17745, #24385 ),
 .UNSPECIFIED., .F., .F.,
 ( 4, 2, 2, 2, 2, 2, 2, 2, 4 ),
 ( 0.000000000000000000, 0.1250000000000000000, 0.2500000000000000000, 0.3750000000000000000, 0.5000000000000000000, 0.6250000000000000000, 0.7500000000000000000, 0.8750000000000000000, 1.000000000000000000 ),
 .UNSPECIFIED. ) ;
#5960 = ORIENTED_EDGE ( 'NONE', *, *, #24424, .F. ) ;
#5961 = DIRECTION ( 'NONE',  ( 1.000000000000000000, 0.000000000000000000, 0.000000000000000000 ) ) ;
#5962 = AXIS2_PLACEMENT_3D ( 'NONE', #25760, #19682, #19255 ) ;
#5963 = DIRECTION ( 'NONE',  ( 1.000000000000000000, 0.000000000000000000, 0.000000000000000000 ) ) ;
#5964 = CARTESIAN_POINT ( 'NONE',  ( 0.1180276236025431108, -0.3257325899126714552, 0.1377952755905513527 ) ) ;
#5965 = EDGE_CURVE ( 'NONE', #14009, #3330, #16665, .T. ) ;
#5966 = LINE ( 'NONE', #1709, #21798 ) ;
#5967 = EDGE_LOOP ( 'NONE', ( #27752, #644 ) ) ;
#5968 = DIRECTION ( 'NONE',  ( 1.000000000000000000, 0.000000000000000000, 0.000000000000000000 ) ) ;
#5969 = DIRECTION ( 'NONE',  ( 1.000000000000000000, 0.000000000000000000, 0.000000000000000000 ) ) ;
#5970 = CARTESIAN_POINT ( 'NONE',  ( 0.02190250779246040100, 0.3346456692913385988, 1.953740157480315043 ) ) ;
#5971 = CARTESIAN_POINT ( 'NONE',  ( -0.5085118447796470598, -0.06699507805605113553, -1.550196850393700920 ) ) ;
#5972 = CYLINDRICAL_SURFACE ( 'NONE', #15485, 0.3722026523000413478 ) ;
#5973 = CARTESIAN_POINT ( 'NONE',  ( -0.4300830224589641260, 0.3772436174784328244, 0.9399606299212598381 ) ) ;
#5974 = CARTESIAN_POINT ( 'NONE',  ( 0.000000000000000000, 0.000000000000000000, -0.07578740157480315376 ) ) ;
#5975 = ORIENTED_EDGE ( 'NONE', *, *, #24525, .F. ) ;
#5976 = PRODUCT_DEFINITION_SHAPE ( 'NONE', 'NONE',  #669 ) ;
#5977 = CARTESIAN_POINT ( 'NONE',  ( -0.09275248786873620255, 0.3460502918090236357, -3.115157480314960647 ) ) ;
#5978 = CIRCLE ( 'NONE', #23117, 0.4692913385826771866 ) ;
#5979 = ORIENTED_EDGE ( 'NONE', *, *, #22943, .T. ) ;
#5980 = CARTESIAN_POINT ( 'NONE',  ( 0.4613045817969895213, 0.2662790972925014876, 1.747047244094487972 ) ) ;
#5981 = EDGE_CURVE ( 'NONE', #5851, #2049, #6284, .T. ) ;
#5982 = EDGE_LOOP ( 'NONE', ( #19905, #19422 ) ) ;
#5983 = AXIS2_PLACEMENT_3D ( 'NONE', #4328, #17184, #19155 ) ;
#5984 = EDGE_CURVE ( 'NONE', #10834, #19874, #22524, .T. ) ;
#5985 = CARTESIAN_POINT ( 'NONE',  ( -0.3707612262533164782, -0.3252100150720257377, -1.550196850393700920 ) ) ;
#5986 = DIRECTION ( 'NONE',  ( 0.000000000000000000, 1.000000000000000000, 0.000000000000000000 ) ) ;
#5987 = CARTESIAN_POINT ( 'NONE',  ( 0.3976891862754212137, 1.133679329692560245, -0.4395307839725697274 ) ) ;
#5988 = CARTESIAN_POINT ( 'NONE',  ( 0.09590060490395689585, 0.1136516277932340530, -0.1968503937007874127 ) ) ;
#5989 = CARTESIAN_POINT ( 'NONE',  ( 0.000000000000000000, 0.000000000000000000, 0.3401574803149606252 ) ) ;
#5990 = B_SPLINE_CURVE_WITH_KNOTS ( 'NONE', 3,
 ( #13119, #21746, #6127, #8879 ),
 .UNSPECIFIED., .F., .F.,
 ( 4, 4 ),
 ( 0.2390783382518553157, 0.2405446243645580073 ),
 .UNSPECIFIED. ) ;
#5991 = ORIENTED_EDGE ( 'NONE', *, *, #18076, .T. ) ;
#5992 = CARTESIAN_POINT ( 'NONE',  ( -0.5511811023622047445, 0.6889763779527560139, 0.000000000000000000 ) ) ;
#5993 = EDGE_LOOP ( 'NONE', ( #15111, #4388, #18053, #21999 ) ) ;
#5994 = CARTESIAN_POINT ( 'NONE',  ( -0.1968503937007874127, -0.07874015748031495954, -0.04546065111729331171 ) ) ;
#5995 = CARTESIAN_POINT ( 'NONE',  ( -0.5905511811023621549, -0.6348133144914153148, -0.8891632684400255782 ) ) ;
#5996 = CARTESIAN_POINT ( 'NONE',  ( -0.3992017438595018564, -0.2298214351608254269, 0.1771653543307087630 ) ) ;
#5997 = DIRECTION ( 'NONE',  ( 0.000000000000000000, 0.000000000000000000, 1.000000000000000000 ) ) ;
#5998 = CARTESIAN_POINT ( 'NONE',  ( 0.2181459867445876555, -0.4514914376998327428, 0.3080453759178627404 ) ) ;
#5999 = ORIENTED_EDGE ( 'NONE', *, *, #22197, .F. ) ;
#6000 = AXIS2_PLACEMENT_3D ( 'NONE', #3567, #6001, #14780 ) ;
#6001 = DIRECTION ( 'NONE',  ( 0.000000000000000000, 0.000000000000000000, 1.000000000000000000 ) ) ;
#6002 = CIRCLE ( 'NONE', #23600, 0.09143349766193348271 ) ;
#6003 = EDGE_LOOP ( 'NONE', ( #20167, #26088, #12946, #27847 ) ) ;
#6004 = EDGE_CURVE ( 'NONE', #27250, #20760, #8800, .T. ) ;
#6005 = CARTESIAN_POINT ( 'NONE',  ( 0.1173917140416251143, -0.4382752542995838052, -1.934055118110236338 ) ) ;
#6007 = CONICAL_SURFACE ( 'NONE', #24934, 0.3726024258163779246, 0.2617993874999969828 ) ;
#6006 = CARTESIAN_POINT ( 'NONE',  ( 0.4351030398461776527, -0.1477428134820240602, -1.928289503579159625 ) ) ;
#6008 = ORIENTED_EDGE ( 'NONE', *, *, #8644, .T. ) ;
#6009 = VERTEX_POINT ( 'NONE', #6970 ) ;
#6010 = CARTESIAN_POINT ( 'NONE',  ( -0.5072939182192724994, -0.4686501608227520155, -0.02272223917426736267 ) ) ;
#6011 = CARTESIAN_POINT ( 'NONE',  ( 0.3574975638436101444, 4.268512490100411279E-17, -3.115157480314960647 ) ) ;
#6012 = CARTESIAN_POINT ( 'NONE',  ( -0.5314960629921260393, -0.03478633594543723700, 1.747047244094488194 ) ) ;
#6013 = ORIENTED_EDGE ( 'NONE', *, *, #16544, .T. ) ;
#6014 = AXIS2_PLACEMENT_3D ( 'NONE', #17406, #17802, #15319 ) ;
#6015 = VERTEX_POINT ( 'NONE', #17564 ) ;
#6016 = CARTESIAN_POINT ( 'NONE',  ( -0.09842519685039370636, 0.2165354330708661457, -3.456364829396325611 ) ) ;
#6017 = CARTESIAN_POINT ( 'NONE',  ( -1.012503259137575512E-16, -0.8267716535433071723, 0.4488188976377953110 ) ) ;
#6018 = VECTOR ( 'NONE', #4606, 39.37007874015748143 ) ;
#6019 = CARTESIAN_POINT ( 'NONE',  ( -0.0005696707463070112927, 0.4606295689977898400, 0.1771653543307085965 ) ) ;
#6020 = ORIENTED_EDGE ( 'NONE', *, *, #3593, .F. ) ;
#6021 = CARTESIAN_POINT ( 'NONE',  ( 0.2669480828848126985, 0.2341512108694336625, 1.953740157480315043 ) ) ;
#6022 = ORIENTED_EDGE ( 'NONE', *, *, #25024, .F. ) ;
#6023 = ORIENTED_EDGE ( 'NONE', *, *, #17691, .T. ) ;
#6024 = AXIS2_PLACEMENT_3D ( 'NONE', #19196, #23324, #18909 ) ;
#6025 = CARTESIAN_POINT ( 'NONE',  ( -0.6257187983968769407, -0.06950490751670782008, -0.2391845094378674264 ) ) ;
#6027 = CARTESIAN_POINT ( 'NONE',  ( -0.4300830224589284878, -0.3772436174784035146, 0.9399606299212598381 ) ) ;
#6026 = DIRECTION ( 'NONE',  ( -0.000000000000000000, -1.000000000000000000, -0.000000000000000000 ) ) ;
#6028 = ( REPRESENTATION_RELATIONSHIP ('NONE','NONE', #12434, #16232 ) REPRESENTATION_RELATIONSHIP_WITH_TRANSFORMATION ( #3642 )SHAPE_REPRESENTATION_RELATIONSHIP( ) ) ;
#6029 = AXIS2_PLACEMENT_3D ( 'NONE', #1545, #8191, #14421 ) ;
#6030 = EDGE_LOOP ( 'NONE', ( #3114, #9421 ) ) ;
#6031 = APPLICATION_CONTEXT ( 'automotive_design' ) ;
#6032 = DIRECTION ( 'NONE',  ( 0.000000000000000000, -1.000000000000000000, 0.000000000000000000 ) ) ;
#6033 = DIRECTION ( 'NONE',  ( -1.000000000000000000, 0.000000000000000000, 0.000000000000000000 ) ) ;
#6034 = CARTESIAN_POINT ( 'NONE',  ( 0.2180698645301770711, -0.2842490391651530390, -3.115157480314960647 ) ) ;
#6035 = CARTESIAN_POINT ( 'NONE',  ( 0.5511811023622047445, 3.414809992080329023E-17, 0.9202755905511811330 ) ) ;
#6036 = CYLINDRICAL_SURFACE ( 'NONE', #14705, 0.5905511811023621549 ) ;
#6037 = CARTESIAN_POINT ( 'NONE',  ( -2.685748425196850164E-17, 0.000000000000000000, -1.934055118110236338 ) ) ;
#6038 = B_SPLINE_CURVE_WITH_KNOTS ( 'NONE', 3,
 ( #13411, #5068, #7068, #323, #9437, #22173 ),
 .UNSPECIFIED., .F., .F.,
 ( 4, 2, 4 ),
 ( 0.5000000000000000000, 0.7500000000000000000, 1.000000000000000000 ),
 .UNSPECIFIED. ) ;
#6039 = VECTOR ( 'NONE', #26191, 39.37007874015748854 ) ;
#6040 = ADVANCED_FACE ( 'NONE', ( #13170 ), #15592, .T. ) ;
#6041 = DIRECTION ( 'NONE',  ( 1.000000000000000000, 0.000000000000000000, 0.000000000000000000 ) ) ;
#6042 = CIRCLE ( 'NONE', #21816, 0.8267716535433071723 ) ;
#6043 = CARTESIAN_POINT ( 'NONE',  ( -0.07870736637777368816, 0.2165354330708661734, -3.212150913388296392 ) ) ;
#6044 = PRODUCT_RELATED_PRODUCT_CATEGORY ( 'part', '', ( #3691 ) ) ;
#6045 = CARTESIAN_POINT ( 'NONE',  ( 0.0006812437162529252389, 0.6577569867597423681, 0.1461456498334882947 ) ) ;
#6046 = EDGE_CURVE ( 'NONE', #24011, #26909, #17569, .T. ) ;
#6047 = ORIENTED_EDGE ( 'NONE', *, *, #11966, .T. ) ;
#6048 = DIRECTION ( 'NONE',  ( 0.000000000000000000, 0.000000000000000000, -1.000000000000000000 ) ) ;
#6049 = CIRCLE ( 'NONE', #21825, 0.3937007874015748254 ) ;
#6050 = CARTESIAN_POINT ( 'NONE',  ( 0.000000000000000000, 0.000000000000000000, 0.3401574803149606252 ) ) ;
#6051 = EDGE_CURVE ( 'NONE', #10335, #14933, #8937, .T. ) ;
#6052 = CIRCLE ( 'NONE', #20937, 0.03937007874015744507 ) ;
#6053 = CARTESIAN_POINT ( 'NONE',  ( 0.000000000000000000, 0.07874015748662489822, 0.000000000000000000 ) ) ;
#6054 = CARTESIAN_POINT ( 'NONE',  ( 0.06957181182499888594, -0.5280699926562973934, 1.747047244094488194 ) ) ;
#6055 = PRODUCT_CONTEXT ( 'NONE', #6560, 'mechanical' ) ;
#6056 = CARTESIAN_POINT ( 'NONE',  ( 0.1490609433615242285, -0.4786070381542913421, 5.861244094488189820E-17 ) ) ;
#6057 = CARTESIAN_POINT ( 'NONE',  ( 0.06699507805370044644, -0.5085118447801416641, 1.766732283464566899 ) ) ;
#6058 = ORIENTED_EDGE ( 'NONE', *, *, #7177, .T. ) ;
#6059 = EDGE_LOOP ( 'NONE', ( #187, #16704, #10312, #27289 ) ) ;
#6060 = CARTESIAN_POINT ( 'NONE',  ( 0.1584254766472199816, -0.3213305936751578717, -3.115157480314960647 ) ) ;
#6061 = ORIENTED_EDGE ( 'NONE', *, *, #20955, .F. ) ;
#6062 = CARTESIAN_POINT ( 'NONE',  ( 0.6241887519799541595, 0.6058146281749130502, 1.119737402735601890E-17 ) ) ;
#6063 = CARTESIAN_POINT ( 'NONE',  ( 0.3561571326799479742, 0.8881672886669704781, -0.6476052193426063974 ) ) ;
#6064 = AXIS2_PLACEMENT_3D ( 'NONE', #8374, #19665, #10761 ) ;
#6065 = CARTESIAN_POINT ( 'NONE',  ( -0.2660793235464223860, 0.2041304421298429095, 1.973425196850393970 ) ) ;
#6066 = VERTEX_POINT ( 'NONE', #2833 ) ;
#6067 = CARTESIAN_POINT ( 'NONE',  ( 0.3912931228432192099, -0.3001918266902123267, -1.550196850393700920 ) ) ;
#6068 = CARTESIAN_POINT ( 'NONE',  ( 0.000000000000000000, 0.6212598425196850238, 0.04842519685039370358 ) ) ;
#6069 = CARTESIAN_POINT ( 'NONE',  ( -0.3713752547280854133, 0.06583429795695157349, 0.1992142436757342316 ) ) ;
#6070 = ORIENTED_EDGE ( 'NONE', *, *, #14605, .T. ) ;
#6071 = ORIENTED_EDGE ( 'NONE', *, *, #1061, .F. ) ;
#6072 = CIRCLE ( 'NONE', #1536, 0.6751968503937006982 ) ;
#6073 = CONTEXT_DEPENDENT_SHAPE_REPRESENTATION ( #27303, #5558 ) ;
#6074 = ORIENTED_EDGE ( 'NONE', *, *, #8060, .T. ) ;
#6075 = DIRECTION ( 'NONE',  ( -0.2588190448135617161, 3.169619147893037226E-17, 0.9659258263664945998 ) ) ;
#6076 = CARTESIAN_POINT ( 'NONE',  ( -0.2078289949484353749, -0.4330237525397954146, 0.2529987172201150769 ) ) ;
#6077 = DIRECTION ( 'NONE',  ( -0.000000000000000000, -0.000000000000000000, 1.000000000000000000 ) ) ;
#6078 = VERTEX_POINT ( 'NONE', #98 ) ;
#6079 = ORIENTED_EDGE ( 'NONE', *, *, #22757, .F. ) ;
#6080 = FACE_OUTER_BOUND ( 'NONE', #25450, .T. ) ;
#6081 = ADVANCED_FACE ( 'NONE', ( #8664 ), #3545, .F. ) ;
#6082 = CIRCLE ( 'NONE', #3339, 0.5570866141732283561 ) ;
#6083 = CARTESIAN_POINT ( 'NONE',  ( 0.000000000000000000, 0.000000000000000000, 0.2574803149606298969 ) ) ;
#6084 = FACE_BOUND ( 'NONE', #239, .T. ) ;
#6085 = CARTESIAN_POINT ( 'NONE',  ( -2.272295064268543552, 0.6488494047548032384, 2.145669291338582862 ) ) ;
#6086 = B_SPLINE_CURVE_WITH_KNOTS ( 'NONE', 3,
 ( #15841, #9468, #21212, #3383, #12158, #25156, #23056, #3831, #25867, #22271, #6515, #10888, #13374, #22000, #11258, #26364, #6527, #4407, #8637, #10899, #481, #12905, #15597, #10176, #7658, #22915, #23063, #25307, #3535, #18794, #3388, #8085, #22762, #14600 ),
 .UNSPECIFIED., .F., .F.,
 ( 4, 2, 2, 2, 2, 2, 2, 2, 2, 2, 2, 2, 2, 2, 2, 2, 4 ),
 ( 0.000000000000000000, 0.03124999999999995837, 0.06249999999999991673, 0.09374999999999987510, 0.1249999999999998335, 0.1562499999999997780, 0.1874999999999997780, 0.2187499999999997502, 0.2499999999999997780, 0.2812499999999997780, 0.3124999999999997780, 0.3437499999999998335, 0.3749999999999998335, 0.4062499999999998335, 0.4374999999999998890, 0.4687500000000000000, 0.5000000000000000000 ),
 .UNSPECIFIED. ) ;
#6087 = CARTESIAN_POINT ( 'NONE',  ( -0.6097469662162354753, -0.1662068818069558362, 0.2254586359451796196 ) ) ;
#6088 = CARTESIAN_POINT ( 'NONE',  ( -0.2309201403895327909, 0.4006498629591503935, -1.928289503579156960 ) ) ;
#6089 = FACE_BOUND ( 'NONE', #20083, .T. ) ;
#6090 = EDGE_CURVE ( 'NONE', #17891, #18606, #13617, .T. ) ;
#6091 = DIRECTION ( 'NONE',  ( 1.000000000000000000, 0.000000000000000000, 0.000000000000000000 ) ) ;
#6092 = CARTESIAN_POINT ( 'NONE',  ( -0.5525004126151165096, 0.09742072959660473541, 0.1771653543307086520 ) ) ;
#6093 = DIRECTION ( 'NONE',  ( 0.000000000000000000, -1.000000000000000000, 0.000000000000000000 ) ) ;
#6094 = VERTEX_POINT ( 'NONE', #26714 ) ;
#6095 = AXIS2_PLACEMENT_3D ( 'NONE', #19887, #2907, #17877 ) ;
#6096 = DIRECTION ( 'NONE',  ( 0.000000000000000000, -1.000000000000000000, 0.000000000000000000 ) ) ;
#6097 = ADVANCED_FACE ( 'NONE', ( #15995 ), #12610, .T. ) ;
#6098 = CARTESIAN_POINT ( 'NONE',  ( 0.1286734528930086607, -0.3545375539099149265, 0.07637630750536809898 ) ) ;
#6099 = B_SPLINE_CURVE_WITH_KNOTS ( 'NONE', 3,
 ( #10720, #166, #3949, #19194, #8332, #4762, #9402, #19753 ),
 .UNSPECIFIED., .F., .F.,
 ( 4, 2, 2, 4 ),
 ( 0.000000000000000000, 0.2500000000000000000, 0.5000000000000000000, 1.000000000000000000 ),
 .UNSPECIFIED. ) ;
#6100 = ORIENTED_EDGE ( 'NONE', *, *, #27239, .T. ) ;
#6101 = CARTESIAN_POINT ( 'NONE',  ( -0.4856708409191258236, -0.1649135259639268325, -1.550196850393700920 ) ) ;
#6102 = DIRECTION ( 'NONE',  ( 0.000000000000000000, 1.000000000000000000, 0.000000000000000000 ) ) ;
#6103 = CARTESIAN_POINT ( 'NONE',  ( 0.000000000000000000, 0.000000000000000000, -0.01377952755905511792 ) ) ;
#6104 = CARTESIAN_POINT ( 'NONE',  ( -0.2442565704126104242, 0.4954197419817720216, 0.9202755905511811330 ) ) ;
#6105 = EDGE_LOOP ( 'NONE', ( #20563, #23978 ) ) ;
#6106 = CIRCLE ( 'NONE', #4296, 0.2952755905511810774 ) ;
#6107 = CARTESIAN_POINT ( 'NONE',  ( 0.000000000000000000, 0.4232283464566928832, 0.1377952755905511861 ) ) ;
#6108 = CARTESIAN_POINT ( 'NONE',  ( 0.000000000000000000, 0.3771653543307086909, -3.278217716535432842E-17 ) ) ;
#6109 = CARTESIAN_POINT ( 'NONE',  ( -0.0002221395201540944610, 0.5322834645669292097, 0.3401599409343964431 ) ) ;
#6110 = CARTESIAN_POINT ( 'NONE',  ( -0.2158067241058057306, -0.4466421405404321088, 0.2989974301043377136 ) ) ;
#6112 = EDGE_CURVE ( 'NONE', #26553, #20265, #14894, .T. ) ;
#6111 = VECTOR ( 'NONE', #1519, 39.37007874015748143 ) ;
#6113 = CARTESIAN_POINT ( 'NONE',  ( -0.3543307086367249448, 4.339299681715786259E-17, -0.1377952755696461029 ) ) ;
#6114 = EDGE_LOOP ( 'NONE', ( #20873, #27817 ) ) ;
#6115 = AXIS2_PLACEMENT_3D ( 'NONE', #23276, #21425, #10395 ) ;
#6116 = ORIENTED_EDGE ( 'NONE', *, *, #617, .T. ) ;
#6117 = CARTESIAN_POINT ( 'NONE',  ( 0.4600326175569787179, -0.2268096725200276775, -1.550196850393700920 ) ) ;
#6118 = EDGE_CURVE ( 'NONE', #12001, #22551, #13472, .T. ) ;
#6119 = CARTESIAN_POINT ( 'NONE',  ( 0.01504182353227358389, 0.2012500529900838608, 0.000000000000000000 ) ) ;
#6120 = CARTESIAN_POINT ( 'NONE',  ( 0.06894484415077314909, -0.05111597790490109150, -0.4724409448818898127 ) ) ;
#6121 = CARTESIAN_POINT ( 'NONE',  ( -0.5708661417322835607, 0.03736310157554031952, 0.9399606299212598381 ) ) ;
#6122 = CARTESIAN_POINT ( 'NONE',  ( -0.2223167940359792594, 0.2657206863494902538, 0.1377952755905513249 ) ) ;
#6123 = CARTESIAN_POINT ( 'NONE',  ( 0.000000000000000000, 0.3937007873309092409, 0.000000000000000000 ) ) ;
#6124 = VERTEX_POINT ( 'NONE', #2403 ) ;
#6125 = CARTESIAN_POINT ( 'NONE',  ( -0.6751968503937006982, 0.000000000000000000, -4.097771653543307347E-17 ) ) ;
#6126 = EDGE_CURVE ( 'NONE', #20180, #27117, #17109, .T. ) ;
#6127 = CARTESIAN_POINT ( 'NONE',  ( -0.0003854097503898040820, 0.4692912202195576032, 0.07637630773773071424 ) ) ;
#6128 = B_SPLINE_CURVE_WITH_KNOTS ( 'NONE', 3,
 ( #27320, #14776, #23382, #16573, #12337, #8392 ),
 .UNSPECIFIED., .F., .F.,
 ( 4, 2, 4 ),
 ( 0.5000000000000000000, 0.7500000000000000000, 1.000000000000000000 ),
 .UNSPECIFIED. ) ;
#6129 = ORIENTED_EDGE ( 'NONE', *, *, #15873, .T. ) ;
#6130 = CIRCLE ( 'NONE', #15600, 0.6299212598425196763 ) ;
#6131 = CARTESIAN_POINT ( 'NONE',  ( 0.3121994997578124154, -0.4069448477569433953, -1.550196850393700920 ) ) ;
#6132 = ORIENTED_EDGE ( 'NONE', *, *, #18406, .T. ) ;
#6133 = CARTESIAN_POINT ( 'NONE',  ( 0.000000000000000000, 0.000000000000000000, 0.2574803149606298969 ) ) ;
#6134 = CIRCLE ( 'NONE', #20997, 0.6299212598425196763 ) ;
#6135 = DIRECTION ( 'NONE',  ( -1.000000000000000000, 0.000000000000000000, 0.000000000000000000 ) ) ;
#6136 = DIRECTION ( 'NONE',  ( 0.000000000000000000, -1.000000000000000000, 0.000000000000000000 ) ) ;
#6137 = CARTESIAN_POINT ( 'NONE',  ( -0.2356240016490478428, -0.4776900717920959383, 1.747047244094487972 ) ) ;
#6138 = CARTESIAN_POINT ( 'NONE',  ( 0.3381532161288250404, 0.3856588814719275615, -1.550196850393701364 ) ) ;
#6139 = CARTESIAN_POINT ( 'NONE',  ( 0.000000000000000000, 0.000000000000000000, 0.02362204724409448786 ) ) ;
#6140 = ORIENTED_EDGE ( 'NONE', *, *, #14071, .T. ) ;
#6141 = CARTESIAN_POINT ( 'NONE',  ( -0.6010693932361863556, -0.5770964849832589394, -0.9615141454542482924 ) ) ;
#6142 = B_SPLINE_CURVE_WITH_KNOTS ( 'NONE', 2,
 ( #24388, #26497, #13510 ),
 .UNSPECIFIED., .F., .F.,
 ( 3, 3 ),
 ( 0.000000000000000000, 1.000000000000000000 ),
 .UNSPECIFIED. ) ;
#6143 = CARTESIAN_POINT ( 'NONE',  ( -0.5692989725251984545, -0.5056979702041203284, -0.9923584033841372776 ) ) ;
#6144 = CARTESIAN_POINT ( 'NONE',  ( -0.03937007874015747977, 0.000000000000000000, 0.000000000000000000 ) ) ;
#6145 = DIRECTION ( 'NONE',  ( 0.000000000000000000, 1.000000000000000000, 0.000000000000000000 ) ) ;
#6146 = CARTESIAN_POINT ( 'NONE',  ( 0.2158067241018476468, -0.4466421405321954752, 0.2989974300877151769 ) ) ;
#6147 = ORIENTED_EDGE ( 'NONE', *, *, #25869, .T. ) ;
#6148 = CIRCLE ( 'NONE', #10635, 0.3771653543307086909 ) ;
#6149 = PRESENTATION_STYLE_ASSIGNMENT (( #21387 ) ) ;
#6150 = EDGE_CURVE ( 'NONE', #18606, #14935, #5840, .T. ) ;
#6151 = CYLINDRICAL_SURFACE ( 'NONE', #6000, 0.4692913385826771866 ) ;
#6152 = ORIENTED_EDGE ( 'NONE', *, *, #19042, .F. ) ;
#6153 = CARTESIAN_POINT ( 'NONE',  ( 0.5869493968219645641, -0.4267795243146149664, 5.226543307086613929E-17 ) ) ;
#6154 = B_SPLINE_CURVE_WITH_KNOTS ( 'NONE', 3,
 ( #16619, #25796, #19152, #25660, #27649, #8563 ),
 .UNSPECIFIED., .F., .F.,
 ( 4, 2, 4 ),
 ( 0.5000000000000000000, 0.7499999999999998890, 1.000000000000000000 ),
 .UNSPECIFIED. ) ;
#6155 = EDGE_CURVE ( 'NONE', #23029, #25669, #5521, .T. ) ;
#6156 = CARTESIAN_POINT ( 'NONE',  ( 0.000000000000000000, 0.000000000000000000, 0.01181102362204724393 ) ) ;
#6157 = CARTESIAN_POINT ( 'NONE',  ( -0.3454440660767217341, 0.3030032861725395210, -1.928289503579147635 ) ) ;
#6158 = EDGE_CURVE ( 'NONE', #10366, #22192, #26418, .T. ) ;
#6159 = AXIS2_PLACEMENT_3D ( 'NONE', #4996, #22663, #3287 ) ;
#6160 = AXIS2_PLACEMENT_3D ( 'NONE', #16630, #22854, #8164 ) ;
#6161 = ORIENTED_EDGE ( 'NONE', *, *, #1708, .F. ) ;
#6162 = ORIENTED_EDGE ( 'NONE', *, *, #24932, .F. ) ;
#6163 = EDGE_LOOP ( 'NONE', ( #23262, #25298 ) ) ;
#6164 = CARTESIAN_POINT ( 'NONE',  ( -0.4609540795476803621, -0.6224706135936574070, -0.1071654190663385853 ) ) ;
#6165 = FACE_OUTER_BOUND ( 'NONE', #15846, .T. ) ;
#6166 = CARTESIAN_POINT ( 'NONE',  ( 0.06957181182499888594, -0.5280699926562973934, 1.747047244094488194 ) ) ;
#6167 = DIRECTION ( 'NONE',  ( 0.000000000000000000, 0.000000000000000000, -1.000000000000000000 ) ) ;
#6168 = ORIENTED_EDGE ( 'NONE', *, *, #1068, .T. ) ;
#6169 = CARTESIAN_POINT ( 'NONE',  ( -0.1610509776512037416, -0.4407912692718771175, 0.07637795275590551769 ) ) ;
#6170 = DIRECTION ( 'NONE',  ( 0.000000000000000000, -1.000000000000000000, 0.000000000000000000 ) ) ;
#6171 = LINE ( 'NONE', #21406, #12454 ) ;
#6172 = CARTESIAN_POINT ( 'NONE',  ( -0.3995939286814633173, 0.1970998888479515987, -1.934055118110236338 ) ) ;
#6173 = ORIENTED_EDGE ( 'NONE', *, *, #10087, .T. ) ;
#6174 = ORIENTED_EDGE ( 'NONE', *, *, #23058, .F. ) ;
#6175 = CARTESIAN_POINT ( 'NONE',  ( -0.5953962971613582233, -0.1370369651175855630, -0.2478037815953649248 ) ) ;
#6176 = CARTESIAN_POINT ( 'NONE',  ( 0.4065144339881338054, -0.2344790234878023627, 0.1992150590373740204 ) ) ;
#6177 = ORIENTED_EDGE ( 'NONE', *, *, #251, .T. ) ;
#6178 = FACE_OUTER_BOUND ( 'NONE', #13209, .T. ) ;
#6179 = CARTESIAN_POINT ( 'NONE',  ( 0.03532354024591720376, -0.8267716535433071723, 0.000000000000000000 ) ) ;
#6180 = AXIS2_PLACEMENT_3D ( 'NONE', #11911, #1189, #9789 ) ;
#6181 = B_SPLINE_CURVE_WITH_KNOTS ( 'NONE', 3,
 ( #10656, #23399, #12643, #21270, #1902, #19277, #10515, #19134, #27768, #4843, #19830, #624, #17697, #13186, #17432, #26050, #15347 ),
 .UNSPECIFIED., .F., .F.,
 ( 4, 2, 2, 1, 2, 2, 2, 2, 4 ),
 ( 0.08984410251848014284, 0.2036135897036702169, 0.2604983332962649833, 0.3173830768888596943, 0.4311525640740497822, 0.5449220512592398702, 0.6586915384444299582, 0.7724610256296200461, 1.000000000000000000 ),
 .UNSPECIFIED. ) ;
#6182 = CARTESIAN_POINT ( 'NONE',  ( -0.2362439534887433856, 0.2693339498142315325, -3.115157480314960647 ) ) ;
#6183 = CARTESIAN_POINT ( 'NONE',  ( 0.000000000000000000, 0.000000000000000000, 0.2374015748031496065 ) ) ;
#6184 = DIRECTION ( 'NONE',  ( 0.000000000000000000, 0.000000000000000000, -1.000000000000000000 ) ) ;
#6185 = CARTESIAN_POINT ( 'NONE',  ( 0.000000000000000000, 0.000000000000000000, -4.330708661417323135 ) ) ;
#6186 = EDGE_CURVE ( 'NONE', #23082, #27011, #26137, .T. ) ;
#6187 = CARTESIAN_POINT ( 'NONE',  ( 0.0005980912172666611815, 0.4999996422861968659, 0.1496602734623769526 ) ) ;
#6188 = CARTESIAN_POINT ( 'NONE',  ( -0.6711032387266713251, -0.1523958994812759926, 0.3401574803149606252 ) ) ;
#6189 = DIRECTION ( 'NONE',  ( 0.000000000000000000, 1.000000000000000000, 0.000000000000000000 ) ) ;
#6190 = DIRECTION ( 'NONE',  ( 1.000000000000000000, 0.000000000000000000, 0.000000000000000000 ) ) ;
#6191 = CARTESIAN_POINT ( 'NONE',  ( 0.000000000000000000, 0.5322834645669292097, 0.06614173228346456601 ) ) ;
#6192 = FACE_OUTER_BOUND ( 'NONE', #22187, .T. ) ;
#6193 = EDGE_LOOP ( 'NONE', ( #16822, #3789, #19449, #4451, #17611 ) ) ;
#6194 = CARTESIAN_POINT ( 'NONE',  ( 0.000000000000000000, 0.000000000000000000, -0.3779527559055118058 ) ) ;
#6195 = DIMENSIONAL_EXPONENTS ( 1.000000000000000000, 0.000000000000000000, 0.000000000000000000, 0.000000000000000000, 0.000000000000000000, 0.000000000000000000, 0.000000000000000000 ) ;
#6196 = FACE_OUTER_BOUND ( 'NONE', #21586, .T. ) ;
#6197 = ORIENTED_EDGE ( 'NONE', *, *, #12888, .F. ) ;
#6198 = AXIS2_PLACEMENT_3D ( 'NONE', #21910, #15561, #23760 ) ;
#6199 = ORIENTED_EDGE ( 'NONE', *, *, #25903, .T. ) ;
#6200 = CARTESIAN_POINT ( 'NONE',  ( 0.2180698645301770711, -0.2842490391651530390, -3.115157480314960647 ) ) ;
#6201 = CARTESIAN_POINT ( 'NONE',  ( -0.1658689444480831165, -0.4574452598412719895, 0.1827409795211070442 ) ) ;
#6202 = ORIENTED_EDGE ( 'NONE', *, *, #17489, .F. ) ;
#6203 = EDGE_CURVE ( 'NONE', #14125, #21357, #24662, .T. ) ;
#6204 = CARTESIAN_POINT ( 'NONE',  ( 0.6397637795275591399, 0.000000000000000000, -0.7874015748031496509 ) ) ;
#6205 = CARTESIAN_POINT ( 'NONE',  ( 0.3175540113612324578, -0.1078280746903944320, 1.973425196850393970 ) ) ;
#6206 = ORIENTED_EDGE ( 'NONE', *, *, #27465, .T. ) ;
#6207 = ADVANCED_FACE ( 'NONE', ( #20515, #19089 ), #15019, .T. ) ;
#6208 = EDGE_LOOP ( 'NONE', ( #23855, #3827, #18468, #9517 ) ) ;
#6209 = CARTESIAN_POINT ( 'NONE',  ( 0.1585706980422246781, 0.4669911931914895176, -1.550196850393700920 ) ) ;
#6210 = DIRECTION ( 'NONE',  ( 0.000000000000000000, 1.000000000000000000, 0.000000000000000000 ) ) ;
#6211 = ORIENTED_EDGE ( 'NONE', *, *, #26649, .T. ) ;
#6212 = ORIENTED_EDGE ( 'NONE', *, *, #12680, .F. ) ;
#6213 = CARTESIAN_POINT ( 'NONE',  ( -0.1643029338972192277, -0.4497088275967213167, 0.1920935997042204635 ) ) ;
#6214 = EDGE_CURVE ( 'NONE', #25955, #13695, #25285, .T. ) ;
#6215 = ( GEOMETRIC_REPRESENTATION_CONTEXT ( 3 ) GLOBAL_UNCERTAINTY_ASSIGNED_CONTEXT ( ( #3085 ) ) GLOBAL_UNIT_ASSIGNED_CONTEXT ( ( #4516, #2925, #13530 ) ) REPRESENTATION_CONTEXT ( 'NONE', 'WORKASPACE' ) ) ;
#6216 = DIRECTION ( 'NONE',  ( 0.000000000000000000, 0.000000000000000000, 1.000000000000000000 ) ) ;
#6217 = DIRECTION ( 'NONE',  ( 0.000000000000000000, 0.000000000000000000, -1.000000000000000000 ) ) ;
#6218 = B_SPLINE_SURFACE_WITH_KNOTS ( 'NONE', 3, 3, ( 
 ( #1778, #15074, #10815, #4321, #4586 ),
 ( #13200, #14807, #10390, #19429, #5279 ),
 ( #22236, #2731, #26605, #2596, #379 ),
 ( #9092, #501, #15748, #20115, #9363 ) ),
 .UNSPECIFIED., .F., .F., .F.,
 ( 4, 4 ),
 ( 4, 1, 4 ),
 ( -0.5999999999999999778, 0.5999999999999999778 ),
 ( 1.887240170904915137, 3.034981381880270224, 4.565302996514080114 ),
 .UNSPECIFIED. ) ;
#6219 = DIRECTION ( 'NONE',  ( -0.000000000000000000, -1.000000000000000000, -0.000000000000000000 ) ) ;
#6220 = CARTESIAN_POINT ( 'NONE',  ( 0.000000000000000000, 0.000000000000000000, 0.09685039370078740717 ) ) ;
#6221 = CARTESIAN_POINT ( 'NONE',  ( -0.05981201256803149457, 1.563633646945708833, 2.027559055118110187 ) ) ;
#6222 = CARTESIAN_POINT ( 'NONE',  ( -0.6042043723480865491, 1.117528104686773327, 0.04027680511324581436 ) ) ;
#6223 = SPHERICAL_SURFACE ( 'NONE', #16451, 0.1003956692913385851 ) ;
#6224 = CARTESIAN_POINT ( 'NONE',  ( -0.09842519685039377575, 0.2165354330708661457, -3.272637795275590733 ) ) ;
#6225 = CARTESIAN_POINT ( 'NONE',  ( 0.6299212598425196763, 0.04921259842519685318, 0.000000000000000000 ) ) ;
#6226 = ORIENTED_EDGE ( 'NONE', *, *, #27695, .T. ) ;
#6227 = ORIENTED_EDGE ( 'NONE', *, *, #22757, .T. ) ;
#6228 = CIRCLE ( 'NONE', #22006, 0.5007874015748031704 ) ;
#6229 = CARTESIAN_POINT ( 'NONE',  ( 0.3268074212154850611, -0.1882834141668338901, 0.07637630750536809898 ) ) ;
#6230 = EDGE_LOOP ( 'NONE', ( #8621, #24988 ) ) ;
#6231 = ADVANCED_FACE ( 'NONE', ( #27558, #6358 ), #16817, .T. ) ;
#6232 = CONICAL_SURFACE ( 'NONE', #374, 0.4626586504047134341, 0.3230892413134545116 ) ;
#6233 = CARTESIAN_POINT ( 'NONE',  ( -0.4600326175569940945, -0.2268096725200247077, -1.550196850393700920 ) ) ;
#6234 = CARTESIAN_POINT ( 'NONE',  ( 0.000000000000000000, 0.000000000000000000, 0.1771653543307086520 ) ) ;
#6235 = CARTESIAN_POINT ( 'NONE',  ( 0.0007882571242852967879, 0.7401570605731624397, 0.2161412452768986248 ) ) ;
#6236 = ADVANCED_FACE ( 'NONE', ( #8470 ), #14991, .T. ) ;
#6237 = CARTESIAN_POINT ( 'NONE',  ( 0.5230301363771324707, 0.1775991818008611500, 0.9202755905511811330 ) ) ;
#6238 = ORIENTED_EDGE ( 'NONE', *, *, #14772, .F. ) ;
#6239 = ADVANCED_FACE ( 'NONE', ( #27085 ), #18437, .T. ) ;
#6240 = DIRECTION ( 'NONE',  ( 1.000000000000000000, 0.000000000000000000, 0.000000000000000000 ) ) ;
#6241 = ORIENTED_EDGE ( 'NONE', *, *, #3506, .T. ) ;
#6242 = CARTESIAN_POINT ( 'NONE',  ( 0.000000000000000000, 0.3937007874015748254, 0.1771653543307086520 ) ) ;
#6243 = ADVANCED_FACE ( 'NONE', ( #25092 ), #14380, .T. ) ;
#6244 = AXIS2_PLACEMENT_3D ( 'NONE', #14121, #9731, #19916 ) ;
#6245 = AXIS2_PLACEMENT_3D ( 'NONE', #10468, #16983, #23494 ) ;
#6246 = VERTEX_POINT ( 'NONE', #7733 ) ;
#6247 = SPHERICAL_SURFACE ( 'NONE', #3103, 0.07677362204724409722 ) ;
#6248 = DIRECTION ( 'NONE',  ( 0.000000000000000000, -1.000000000000000000, 0.000000000000000000 ) ) ;
#6249 = ORIENTED_EDGE ( 'NONE', *, *, #12698, .T. ) ;
#6250 = CARTESIAN_POINT ( 'NONE',  ( 0.3346456692913385988, 0.000000000000000000, 1.953740157480315043 ) ) ;
#6251 = CARTESIAN_POINT ( 'NONE',  ( 0.5905511811023621549, 0.3346456692913385988, 0.000000000000000000 ) ) ;
#6252 = CARTESIAN_POINT ( 'NONE',  ( -4.821283464566928349E-18, 0.000000000000000000, -0.3779527559055118058 ) ) ;
#6253 = DIRECTION ( 'NONE',  ( -1.000000000000000000, 0.000000000000000000, 0.000000000000000000 ) ) ;
#6254 = CARTESIAN_POINT ( 'NONE',  ( -0.5476281405333571772, -0.07214854559198842499, 0.9399606299212598381 ) ) ;
#6255 = AXIS2_PLACEMENT_3D ( 'NONE', #5528, #14149, #16527 ) ;
#6256 = VERTEX_POINT ( 'NONE', #16209 ) ;
#6257 = CARTESIAN_POINT ( 'NONE',  ( 0.000000000000000000, 0.000000000000000000, -3.278217716535432842E-17 ) ) ;
#6258 = ORIENTED_EDGE ( 'NONE', *, *, #6939, .T. ) ;
#6259 = ADVANCED_FACE ( 'NONE', ( #5469 ), #16803, .F. ) ;
#6260 = AXIS2_PLACEMENT_3D ( 'NONE', #19894, #22427, #15532 ) ;
#6261 = CARTESIAN_POINT ( 'NONE',  ( 0.5118110236220473341, 0.03349795313024165472, -1.550196850393700920 ) ) ;
#6262 = CARTESIAN_POINT ( 'NONE',  ( 0.3771675965698876309, -0.4301570366551953351, 0.9399606299212600602 ) ) ;
#6263 = DIRECTION ( 'NONE',  ( -1.000000000000000000, 0.000000000000000000, 0.000000000000000000 ) ) ;
#6264 = AXIS2_PLACEMENT_3D ( 'NONE', #12898, #21525, #2027 ) ;
#6265 = DIRECTION ( 'NONE',  ( -1.000000000000000000, 0.000000000000000000, 0.000000000000000000 ) ) ;
#6266 = CARTESIAN_POINT ( 'NONE',  ( -0.5043892184459256578, -0.1711665596935614542, 1.747047244094487972 ) ) ;
#6267 = EDGE_CURVE ( 'NONE', #12664, #22294, #20259, .T. ) ;
#6268 = CARTESIAN_POINT ( 'NONE',  ( 0.06690352886846342995, 0.5085315017395506398, -1.550196850393700920 ) ) ;
#6269 = DIRECTION ( 'NONE',  ( 1.000000000000000000, 0.000000000000000000, 0.000000000000000000 ) ) ;
#6270 = ORIENTED_EDGE ( 'NONE', *, *, #20896, .F. ) ;
#6271 = FACE_OUTER_BOUND ( 'NONE', #4087, .T. ) ;
#6272 = AXIS2_PLACEMENT_3D ( 'NONE', #11216, #23948, #9220 ) ;
#6273 = DIRECTION ( 'NONE',  ( -1.000000000000000000, 0.000000000000000000, 0.000000000000000000 ) ) ;
#6274 = CARTESIAN_POINT ( 'NONE',  ( 0.2720459371704843088, 0.3242117229735830830, 0.1377952755905511861 ) ) ;
#6275 = FACE_OUTER_BOUND ( 'NONE', #10466, .T. ) ;
#6276 = VERTEX_POINT ( 'NONE', #5900 ) ;
#6277 = LINE ( 'NONE', #3871, #10048 ) ;
#6278 = VERTEX_POINT ( 'NONE', #3610 ) ;
#6279 = FACE_OUTER_BOUND ( 'NONE', #9688, .T. ) ;
#6280 = CARTESIAN_POINT ( 'NONE',  ( -0.4302903874097571135, -0.2491168502853802758, 0.1140743250948484666 ) ) ;
#6281 = ADVANCED_FACE ( 'NONE', ( #12240 ), #3186, .T. ) ;
#6282 = PRODUCT_DEFINITION_CONTEXT ( 'detailed design', #13230, 'design' ) ;
#6283 = CARTESIAN_POINT ( 'NONE',  ( 0.4069519308877018182, 0.2006393256663585589, -1.934055118110236338 ) ) ;
#6284 = CIRCLE ( 'NONE', #8533, 1.131889763779527547 ) ;
#6285 = VECTOR ( 'NONE', #11721, 39.37007874015748143 ) ;
#6286 = B_SPLINE_CURVE_WITH_KNOTS ( 'NONE', 3,
 ( #819, #7171, #26950, #15793, #9408, #24260 ),
 .UNSPECIFIED., .F., .F.,
 ( 4, 2, 4 ),
 ( 0.3864984308775630262, 0.3881911340211379735, 0.3898838371647110335 ),
 .UNSPECIFIED. ) ;
#6287 = VERTEX_POINT ( 'NONE', #10118 ) ;
#6288 = ORIENTED_EDGE ( 'NONE', *, *, #2195, .F. ) ;
#6289 = CARTESIAN_POINT ( 'NONE',  ( -0.4881018399981850719, -0.5317657191589535426, -0.05369922615894921064 ) ) ;
#6290 = ( LENGTH_UNIT ( ) NAMED_UNIT ( * ) SI_UNIT ( $, .METRE. ) ) ;
#6291 = CARTESIAN_POINT ( 'NONE',  ( 0.1378076643338767004, -0.5144970376935934508, 1.747047244094488194 ) ) ;
#6292 = CARTESIAN_POINT ( 'NONE',  ( -0.5708661417322835607, -1.112204724409448842, 0.000000000000000000 ) ) ;
#6293 = ORIENTED_EDGE ( 'NONE', *, *, #24317, .F. ) ;
#6294 = EDGE_CURVE ( 'NONE', #5784, #2317, #11684, .T. ) ;
#6295 = DIRECTION ( 'NONE',  ( 0.000000000000000000, 0.000000000000000000, 1.000000000000000000 ) ) ;
#6296 = DIRECTION ( 'NONE',  ( -0.000000000000000000, -0.000000000000000000, 1.000000000000000000 ) ) ;
#6297 = CARTESIAN_POINT ( 'NONE',  ( -0.2227473777833936797, 0.3858850602362957072, -1.934055118110236338 ) ) ;
#6298 = ADVANCED_FACE ( 'NONE', ( #24808 ), #21203, .F. ) ;
#6299 = ORIENTED_EDGE ( 'NONE', *, *, #18379, .F. ) ;
#6300 = CARTESIAN_POINT ( 'NONE',  ( 0.1775730735577447927, -0.3074993854542728555, 1.953740157480315043 ) ) ;
#6301 = CARTESIAN_POINT ( 'NONE',  ( -0.5628483367911055746, -0.2097809568884774767, -0.2636329226663323144 ) ) ;
#6302 = AXIS2_PLACEMENT_3D ( 'NONE', #12976, #17365, #8604 ) ;
#6303 = DIRECTION ( 'NONE',  ( -1.000000000000000000, 0.000000000000000000, 0.000000000000000000 ) ) ;
#6304 = CARTESIAN_POINT ( 'NONE',  ( -0.2529800193559321730, -0.5131133041954082374, 0.9399606299212598381 ) ) ;
#6305 = AXIS2_PLACEMENT_3D ( 'NONE', #8029, #20731, #1376 ) ;
#6306 = DIRECTION ( 'NONE',  ( 0.000000000000000000, 0.000000000000000000, 1.000000000000000000 ) ) ;
#6307 = ORIENTED_EDGE ( 'NONE', *, *, #18039, .T. ) ;
#6308 = ORIENTED_EDGE ( 'NONE', *, *, #23058, .T. ) ;
#6309 = DIRECTION ( 'NONE',  ( 1.000000000000000000, 0.000000000000000000, 0.000000000000000000 ) ) ;
#6310 = DIRECTION ( 'NONE',  ( 0.7660444431189777914, -0.6427876096865396960, 0.000000000000000000 ) ) ;
#6311 = CARTESIAN_POINT ( 'NONE',  ( 0.1200583359873108324, 0.3535721684717922364, -3.115157480314960647 ) ) ;
#6312 = FACE_OUTER_BOUND ( 'NONE', #15378, .T. ) ;
#6313 = DIRECTION ( 'NONE',  ( -1.000000000000000000, -1.224646799147356165E-16, 0.000000000000000000 ) ) ;
#6314 = CARTESIAN_POINT ( 'NONE',  ( 0.0003954787107570765094, 0.5007872847596378518, 0.2574819596263889787 ) ) ;
#6315 = DIRECTION ( 'NONE',  ( 0.000000000000000000, 0.000000000000000000, 1.000000000000000000 ) ) ;
#6316 = CARTESIAN_POINT ( 'NONE',  ( 0.3935368318888682881, -0.3024344094364739832, -1.569881889763779625 ) ) ;
#6317 = CARTESIAN_POINT ( 'NONE',  ( -0.5905511811023621549, -0.4526313213353566622, -0.9943460912301791410 ) ) ;
#6318 = CARTESIAN_POINT ( 'NONE',  ( -0.4152525734086684461, 0.3642352168757148068, 0.9202755905511811330 ) ) ;
#6319 = CIRCLE ( 'NONE', #27538, 0.4173228346456693272 ) ;
#6320 = DIRECTION ( 'NONE',  ( 0.000000000000000000, 1.000000000000000000, 0.000000000000000000 ) ) ;
#6321 = CARTESIAN_POINT ( 'NONE',  ( 0.5375739373539409893, 0.4296723508511047229, 0.1322834645669291320 ) ) ;
#6322 = ORIENTED_EDGE ( 'NONE', *, *, #20618, .T. ) ;
#6323 = VECTOR ( 'NONE', #1926, 39.37007874015748143 ) ;
#6324 = CARTESIAN_POINT ( 'NONE',  ( -0.7874015748031496509, 0.6226544199590670070, -0.5245967315940827103 ) ) ;
#6325 = SHAPE_DEFINITION_REPRESENTATION ( #7998, #3575 ) ;
#6326 = CARTESIAN_POINT ( 'NONE',  ( -0.4600326175560602304, -0.2268096725222347454, 1.766732283464566899 ) ) ;
#6327 = EDGE_LOOP ( 'NONE', ( #22336, #8855, #27429, #8820 ) ) ;
#6328 = CIRCLE ( 'NONE', #13981, 0.1299232283464566984 ) ;
#6330 = CARTESIAN_POINT ( 'NONE',  ( 0.1584254766472226184, 0.3213305936751399972, -3.115157480314960647 ) ) ;
#6329 = DIRECTION ( 'NONE',  ( 0.000000000000000000, 0.000000000000000000, 1.000000000000000000 ) ) ;
#6331 = CARTESIAN_POINT ( 'NONE',  ( 0.3680051700917441604, 0.000000000000000000, 0.000000000000000000 ) ) ;
#6332 = VERTEX_POINT ( 'NONE', #18146 ) ;
#6333 = CARTESIAN_POINT ( 'NONE',  ( -0.3131893444219968625, 0.3723335979320288591, 0.2467937632980442275 ) ) ;
#6334 = B_SPLINE_CURVE_WITH_KNOTS ( 'NONE', 3,
 ( #11559, #9023, #19641, #20175, #19908, #7055 ),
 .UNSPECIFIED., .F., .F.,
 ( 4, 2, 4 ),
 ( 0.000000000000000000, 0.2500000000000000000, 0.5000000000000000000 ),
 .UNSPECIFIED. ) ;
#6335 = EDGE_CURVE ( 'NONE', #5588, #2791, #4042, .T. ) ;
#6336 = CARTESIAN_POINT ( 'NONE',  ( 0.3007905576423843819, -0.1482986320106508549, 1.973425196850393970 ) ) ;
#6337 = ORIENTED_EDGE ( 'NONE', *, *, #4876, .T. ) ;
#6338 = SHAPE_REPRESENTATION ( 'Cam Follower', ( #11588 ), #22004 ) ;
#6339 = ORIENTED_EDGE ( 'NONE', *, *, #22252, .T. ) ;
#6340 = ADVANCED_FACE ( 'NONE', ( #11819 ), #20435, .F. ) ;
#6341 = CARTESIAN_POINT ( 'NONE',  ( -0.3001918266901933974, 0.3912931228432126596, -1.550196850393700920 ) ) ;
#6342 = FACE_BOUND ( 'NONE', #6230, .T. ) ;
#6343 = ORIENTED_EDGE ( 'NONE', *, *, #23489, .T. ) ;
#6344 = ORIENTED_EDGE ( 'NONE', *, *, #7766, .F. ) ;
#6345 = ORIENTED_EDGE ( 'NONE', *, *, #6623, .T. ) ;
#6346 = CIRCLE ( 'NONE', #22111, 0.3126261861498082495 ) ;
#6347 = AXIS2_PLACEMENT_3D ( 'NONE', #26823, #11849, #7473 ) ;
#6348 = CARTESIAN_POINT ( 'NONE',  ( 2.632951206231566310, 0.9448818897637796255, -0.1308464566929134210 ) ) ;
#6349 = CARTESIAN_POINT ( 'NONE',  ( -0.09842519685039370636, 0.2991866959364303802, -3.548228346456693050 ) ) ;
#6350 = CARTESIAN_POINT ( 'NONE',  ( 0.4790936880891605854, 0.08507591033000294622, 0.1827409795187460162 ) ) ;
#6351 = ORIENTED_EDGE ( 'NONE', *, *, #20587, .F. ) ;
#6352 = AXIS2_PLACEMENT_3D ( 'NONE', #16420, #18080, #5549 ) ;
#6353 = CARTESIAN_POINT ( 'NONE',  ( -0.3338887748335570560, 0.000000000000000000, -1.052618110236220428 ) ) ;
#6354 = EDGE_CURVE ( 'NONE', #12205, #18210, #25077, .T. ) ;
#6355 = CARTESIAN_POINT ( 'NONE',  ( 0.9840686206212204690, -2.925196850393700920, -0.6496062814238976468 ) ) ;
#6356 = CARTESIAN_POINT ( 'NONE',  ( 0.06441914069860958658, 0.4921259842519684624, -1.569881889763779625 ) ) ;
#6357 = DIRECTION ( 'NONE',  ( -1.000000000000000000, 0.000000000000000000, 0.000000000000000000 ) ) ;
#6358 = FACE_BOUND ( 'NONE', #9068, .T. ) ;
#6359 = CARTESIAN_POINT ( 'NONE',  ( 0.07870736599821760715, 0.2165354330708661457, -3.212150913008740449 ) ) ;
#6360 = VERTEX_POINT ( 'NONE', #11965 ) ;
#6361 = EDGE_CURVE ( 'NONE', #17458, #16146, #16682, .T. ) ;
#6362 = CARTESIAN_POINT ( 'NONE',  ( -0.4092416079569000109, 0.000000000000000000, -0.05856299212598425896 ) ) ;
#6363 = CARTESIAN_POINT ( 'NONE',  ( -0.3661417322834645272, -0.4724409448818898127, 0.9265594366467145848 ) ) ;
#6364 = VERTEX_POINT ( 'NONE', #17318 ) ;
#6365 = VECTOR ( 'NONE', #2338, 39.37007874015748143 ) ;
#6366 = DIRECTION ( 'NONE',  ( 0.000000000000000000, 0.000000000000000000, 1.000000000000000000 ) ) ;
#6367 = CARTESIAN_POINT ( 'NONE',  ( 0.2956505864974371400, 0.3532288989643546651, 0.1771653543307085410 ) ) ;
#6368 = CARTESIAN_POINT ( 'NONE',  ( 0.2442565704126475612, 0.4954197419817565895, 0.9202755905511811330 ) ) ;
#6369 = DIMENSIONAL_EXPONENTS ( 1.000000000000000000, 0.000000000000000000, 0.000000000000000000, 0.000000000000000000, 0.000000000000000000, 0.000000000000000000, 0.000000000000000000 ) ;
#6370 = ORIENTED_EDGE ( 'NONE', *, *, #25909, .F. ) ;
#6371 = LINE ( 'NONE', #4528, #13581 ) ;
#6372 = ORIENTED_EDGE ( 'NONE', *, *, #5207, .F. ) ;
#6373 = DIRECTION ( 'NONE',  ( 0.000000000000000000, 0.000000000000000000, 1.000000000000000000 ) ) ;
#6374 = DIRECTION ( 'NONE',  ( 0.000000000000000000, 0.000000000000000000, 1.000000000000000000 ) ) ;
#6375 = DIRECTION ( 'NONE',  ( 0.000000000000000000, 0.000000000000000000, -1.000000000000000000 ) ) ;
#6376 = CARTESIAN_POINT ( 'NONE',  ( 0.3606190329934327310, 0.4297690281277732338, 0.1771653543307086520 ) ) ;
#6377 = EDGE_CURVE ( 'NONE', #8989, #11425, #16909, .T. ) ;
#6378 = VERTEX_POINT ( 'NONE', #16763 ) ;
#6379 = CARTESIAN_POINT ( 'NONE',  ( 0.000000000000000000, 0.000000000000000000, 0.1992125984251968684 ) ) ;
#6380 = CARTESIAN_POINT ( 'NONE',  ( -0.0004986409324254199252, 0.3484797321232486755, 0.1589462317930222524 ) ) ;
#6381 = DIRECTION ( 'NONE',  ( 0.000000000000000000, 0.000000000000000000, 1.000000000000000000 ) ) ;
#6382 = CARTESIAN_POINT ( 'NONE',  ( 0.6119360453657027854, 0.1072290460172409393, 0.2574803149606298969 ) ) ;
#6383 = LINE ( 'NONE', #6119, #722 ) ;
#6384 = DIRECTION ( 'NONE',  ( 1.000000000000000000, 0.000000000000000000, 0.000000000000000000 ) ) ;
#6385 = EDGE_CURVE ( 'NONE', #17999, #18223, #25936, .T. ) ;
#6386 = CONICAL_SURFACE ( 'NONE', #27603, 0.5511811023268710086, 0.7853981642949031672 ) ;
#6387 = CIRCLE ( 'NONE', #9497, 0.01181102362204730985 ) ;
#6388 = STYLED_ITEM ( 'NONE', ( #5874 ), #12535 ) ;
#6389 = DIRECTION ( 'NONE',  ( 0.000000000000000000, 0.000000000000000000, -1.000000000000000000 ) ) ;
#6390 = EDGE_LOOP ( 'NONE', ( #20404, #3441 ) ) ;
#6391 = CARTESIAN_POINT ( 'NONE',  ( 0.5511811023622048555, -0.03607471876262468430, 0.9399606299212598381 ) ) ;
#6392 = AXIS2_PLACEMENT_3D ( 'NONE', #25997, #19494, #9028 ) ;
#6393 = DIRECTION ( 'NONE',  ( 0.000000000000000000, 0.000000000000000000, -1.000000000000000000 ) ) ;
#6394 = FACE_OUTER_BOUND ( 'NONE', #18086, .T. ) ;
#6395 = ORIENTED_EDGE ( 'NONE', *, *, #22413, .T. ) ;
#6396 = CARTESIAN_POINT ( 'NONE',  ( -0.02345921195965510950, 0.3574961452116666161, -3.115157480314960647 ) ) ;
#6397 = ADVANCED_FACE ( 'NONE', ( #2201, #1645 ), #2064, .T. ) ;
#6398 = EDGE_LOOP ( 'NONE', ( #12982, #3707, #22746, #3158 ) ) ;
#6399 = ADVANCED_FACE ( 'NONE', ( #19295, #25521 ), #25797, .T. ) ;
#6400 = EDGE_LOOP ( 'NONE', ( #14006, #9282, #3718, #18640, #19761, #26637 ) ) ;
#6401 = AXIS2_PLACEMENT_3D ( 'NONE', #11778, #20397, #18398 ) ;
#6402 = CARTESIAN_POINT ( 'NONE',  ( -0.4856708409191340392, 0.1649135259639384898, -1.550196850393700920 ) ) ;
#6403 = FACE_OUTER_BOUND ( 'NONE', #12783, .T. ) ;
#6404 = DIRECTION ( 'NONE',  ( 1.000000000000000000, 0.000000000000000000, 0.000000000000000000 ) ) ;
#6405 = FACE_BOUND ( 'NONE', #17549, .T. ) ;
#6406 = CYLINDRICAL_SURFACE ( 'NONE', #16033, 0.3937007874015748254 ) ;
#6407 = ORIENTED_EDGE ( 'NONE', *, *, #24317, .T. ) ;
#6408 = VECTOR ( 'NONE', #23622, 39.37007874015748143 ) ;
#6409 = FACE_OUTER_BOUND ( 'NONE', #7791, .T. ) ;
#6410 = DIRECTION ( 'NONE',  ( 0.000000000000000000, 0.000000000000000000, -1.000000000000000000 ) ) ;
#6411 = CARTESIAN_POINT ( 'NONE',  ( -0.3996755081322724834, 0.4756294029998802686, 0.2574819594177531479 ) ) ;
#6412 = ORIENTED_EDGE ( 'NONE', *, *, #4099, .T. ) ;
#6413 = EDGE_CURVE ( 'NONE', #11904, #12816, #22540, .T. ) ;
#6414 = ADVANCED_FACE ( 'NONE', ( #15080 ), #21288, .T. ) ;
#6415 = DIRECTION ( 'NONE',  ( 1.000000000000000000, 0.000000000000000000, 0.000000000000000000 ) ) ;
#6416 = ORIENTED_EDGE ( 'NONE', *, *, #25747, .T. ) ;
#6417 = CARTESIAN_POINT ( 'NONE',  ( -0.2180862235769436830, 0.4423390553432706707, -1.550196850393700920 ) ) ;
#6418 = CARTESIAN_POINT ( 'NONE',  ( -0.3411003281197191872, -0.2991932138496762317, -1.934055118110236338 ) ) ;
#6419 = ADVANCED_FACE ( 'NONE', ( #10676, #12800 ), #27785, .T. ) ;
#6420 = CIRCLE ( 'NONE', #24435, 0.4606299212598425341 ) ;
#6421 = ADVANCED_FACE ( 'NONE', ( #3906 ), #14813, .F. ) ;
#6422 = CARTESIAN_POINT ( 'NONE',  ( 0.000000000000000000, 0.000000000000000000, 0.3401574803149606252 ) ) ;
#6423 = TOROIDAL_SURFACE ( 'NONE', #16342, 0.5241918773311228241, 0.01377952755905511792 ) ;
#6424 = ORIENTED_EDGE ( 'NONE', *, *, #4318, .T. ) ;
#6425 = CARTESIAN_POINT ( 'NONE',  ( -0.5355664161054535244, -0.4296723638627480413, 0.1626757613542834380 ) ) ;
#6426 = DIRECTION ( 'NONE',  ( -1.000000000000000000, 0.000000000000000000, 0.000000000000000000 ) ) ;
#6427 = CARTESIAN_POINT ( 'NONE',  ( -0.4895436826823449938, 0.08692528595285195503, 0.1140743250914997425 ) ) ;
#6428 = ORIENTED_EDGE ( 'NONE', *, *, #16585, .F. ) ;
#6429 = LINE ( 'NONE', #18844, #27794 ) ;
#6430 = CARTESIAN_POINT ( 'NONE',  ( 0.09590060490395689585, 0.2273032555864669124, 0.000000000000000000 ) ) ;
#6431 = B_SPLINE_SURFACE_WITH_KNOTS ( 'NONE', 2, 3, ( 
 ( #3489, #10273, #24682, #10001, #18317, #5344, #7611, #13967, #27244, #22579, #20459, #925, #13769, #2034, #26932, #5028, #12089, #24516, #7571, #802, #13647, #5313, #14229, #24799, #22264, #5164, #1230, #13791, #11955, #22412, #2897, #18429, #3314, #9535, #1090, #18137, #9828, #27076, #22835, #7724, #24938, #20428, #5600, #3460, #20712, #1356, #3033, #16058, #13936, #22550, #18567, #3177, #9687, #11810, #2361, #12326, #27745, #4852, #15616, #19426, #6852, #17171, #21965, #21826, #25786, #22093 ),
 ( #26194, #2592, #19840, #9089, #10809, #6716, #21546, #17440, #17305, #25924, #15201, #23812, #15354, #13066, #23946, #4582, #18391, #14190, #14043, #22652, #22792, #3416, #13749, #20109, #9794, #9219, #13895, #11772, #17840, #26458, #7121, #15745, #11494, #22230, #766, #18093, #9646, #2856, #16018, #26886, #9356, #5126, #7393, #11918, #20249, #9498, #17961, #7250, #26599, #26738, #15869, #24761, #24474, #20537, #22372, #2994, #11627, #24616, #5274, #1052, #22514, #5425, #1194, #20554, #10086, #27477 ),
 ( #25204, #8122, #16728, #9667, #3878, #26905, #18694, #21111, #13733, #24063, #9339, #13453, #22355, #17945, #19822, #4697, #21952, #2577, #22076, #750, #2709, #896, #11341, #24332, #13592, #3693, #22814, #27054, #22669, #21670, #2300, #19548, #14785, #21254, #14643, #19122, #6006, #23245, #12496, #4694, #17568, #6975, #22072, #26180, #22349, #13320, #2703, #22209, #27017, #5076, #24993, #22460, #20344, #24492, #7007, #5140, #24228, #16035, #24632, #11788, #8603, #17224, #13483, #20421, #13638, #9527 ) ),
 .UNSPECIFIED., .F., .T., .F.,
 ( 3, 3 ),
 ( 4, 2, 2, 2, 2, 2, 2, 2, 2, 2, 2, 2, 2, 2, 2, 2, 2, 2, 2, 2, 2, 2, 2, 2, 2, 2, 2, 2, 2, 2, 2, 2, 4 ),
 ( 0.000000000000000000, 1.000000000000000000 ),
 ( 0.000000000000000000, 0.1963495408493620697, 0.3926990816987241395, 0.5890486225480862092, 0.7853981633974482790, 0.9817477042468103487, 1.178097245096172418, 1.374446785945534488, 1.570796326794896558, 1.767145867644258628, 1.963495408493620697, 2.159844949342982545, 2.356194490192344837, 2.552544031041707129, 2.748893571891068976, 2.945243112740430824, 3.141592653589793116, 3.337942194439155408, 3.534291735288517255, 3.730641276137879103, 3.926990816987241395, 4.123340357836603687, 4.319689898685965090, 4.516039439535327382, 4.712388980384689674, 4.908738521234051966, 5.105088062083414258, 5.301437602932775661, 5.497787143782137953, 5.694136684631500245, 5.890486225480861648, 6.086835766330223940, 6.283185307179586232 ),
 .UNSPECIFIED. ) ;
#6432 = CARTESIAN_POINT ( 'NONE',  ( 0.3534612032199636600, 0.2712680014832398734, -1.934055118110236338 ) ) ;
#6433 = VECTOR ( 'NONE', #16014, 39.37007874015748143 ) ;
#6434 = FACE_OUTER_BOUND ( 'NONE', #12541, .T. ) ;
#6435 = EDGE_CURVE ( 'NONE', #22985, #11373, #9913, .T. ) ;
#6436 = ORIENTED_EDGE ( 'NONE', *, *, #12114, .T. ) ;
#6437 = CARTESIAN_POINT ( 'NONE',  ( -0.6366897297587940097, -0.04473345904607178153, -0.2370953701923842472 ) ) ;
#6438 = CARTESIAN_POINT ( 'NONE',  ( 0.1532705055535415473, -0.7132778159795964967, -0.1710911351452818752 ) ) ;
#6439 = ORIENTED_EDGE ( 'NONE', *, *, #18603, .F. ) ;
#6440 = DIRECTION ( 'NONE',  ( 0.000000000000000000, 1.000000000000000000, 0.000000000000000000 ) ) ;
#6441 = CARTESIAN_POINT ( 'NONE',  ( -0.2462256503456003442, -0.2807137536170363767, -3.115157480314960647 ) ) ;
#6442 = CARTESIAN_POINT ( 'NONE',  ( -0.09842519685039370636, 0.2165354330708661457, -3.548228346456693050 ) ) ;
#6443 = DIRECTION ( 'NONE',  ( 0.000000000000000000, 0.000000000000000000, -1.000000000000000000 ) ) ;
#6444 = FACE_OUTER_BOUND ( 'NONE', #25099, .T. ) ;
#6445 = DIRECTION ( 'NONE',  ( 0.000000000000000000, -1.000000000000000000, 0.000000000000000000 ) ) ;
#6446 = CARTESIAN_POINT ( 'NONE',  ( 0.4165721057576322606, 0.3313508221749649763, 0.1322834645669291320 ) ) ;
#6447 = EDGE_CURVE ( 'NONE', #19912, #4078, #8564, .T. ) ;
#6448 = EDGE_CURVE ( 'NONE', #14336, #27195, #10811, .T. ) ;
#6449 = ADVANCED_FACE ( 'NONE', ( #4327 ), #25375, .T. ) ;
#6450 = VECTOR ( 'NONE', #9825, 39.37007874015748143 ) ;
#6451 = VERTEX_POINT ( 'NONE', #14673 ) ;
#6452 = DIRECTION ( 'NONE',  ( -0.9659258263664939337, 0.2588190448135644917, 3.169619147893071122E-17 ) ) ;
#6453 = AXIS2_PLACEMENT_3D ( 'NONE', #26750, #24486, #18401 ) ;
#6454 = VERTEX_POINT ( 'NONE', #23277 ) ;
#6455 = DIRECTION ( 'NONE',  ( 1.000000000000000000, 0.000000000000000000, 0.000000000000000000 ) ) ;
#6456 = CARTESIAN_POINT ( 'NONE',  ( 0.4563437505067101663, 0.07988585396536060368, 0.1494804571663867210 ) ) ;
#6457 = APPLICATION_PROTOCOL_DEFINITION ( 'draft international standard', 'automotive_design', 1998, #17041 ) ;
#6458 = CARTESIAN_POINT ( 'NONE',  ( -0.1649135259617057203, -0.4856708409200641841, 1.766732283464566899 ) ) ;
#6459 = EDGE_CURVE ( 'NONE', #478, #14228, #5146, .T. ) ;
#6460 = CARTESIAN_POINT ( 'NONE',  ( -0.3855916753051391033, -0.3382184156731863900, 1.747047244094488194 ) ) ;
#6461 = CARTESIAN_POINT ( 'NONE',  ( -0.4527559055118110520, 0.000000000000000000, 0.000000000000000000 ) ) ;
#6462 = ORIENTED_EDGE ( 'NONE', *, *, #11193, .F. ) ;
#6463 = ORIENTED_EDGE ( 'NONE', *, *, #23730, .T. ) ;
#6465 = CARTESIAN_POINT ( 'NONE',  ( 0.02339816079119036787, -0.3574975638436101444, -3.115157480314960647 ) ) ;
#6464 = CARTESIAN_POINT ( 'NONE',  ( -0.6339803004441102452, 0.1124719464476266473, 0.1183902030382474879 ) ) ;
#6466 = EDGE_LOOP ( 'NONE', ( #19788, #21058, #3858, #5051, #27315 ) ) ;
#6467 = CARTESIAN_POINT ( 'NONE',  ( 0.000000000000000000, 0.000000000000000000, 0.6299212598425196763 ) ) ;
#6468 = ORIENTED_EDGE ( 'NONE', *, *, #24717, .F. ) ;
#6469 = CARTESIAN_POINT ( 'NONE',  ( 0.3976891862754212137, 0.9951575781684135480, -0.5144425584461574941 ) ) ;
#6470 = CARTESIAN_POINT ( 'NONE',  ( -0.2660793235464258277, -0.2041304421298378857, 1.973425196850393970 ) ) ;
#6471 = EDGE_CURVE ( 'NONE', #5795, #7963, #13561, .T. ) ;
#6472 = EDGE_LOOP ( 'NONE', ( #24744, #21279, #20965, #19101, #24711, #8476 ) ) ;
#6473 = EDGE_LOOP ( 'NONE', ( #11151, #3057, #6307, #14316 ) ) ;
#6474 = DIRECTION ( 'NONE',  ( -1.000000000000000000, 0.000000000000000000, 0.000000000000000000 ) ) ;
#6475 = CARTESIAN_POINT ( 'NONE',  ( -1.928513779527558736E-17, 0.000000000000000000, -0.4448818897637791814 ) ) ;
#6476 = ORIENTED_EDGE ( 'NONE', *, *, #25477, .F. ) ;
#6477 = VERTEX_POINT ( 'NONE', #24358 ) ;
#6478 = ORIENTED_EDGE ( 'NONE', *, *, #284, .F. ) ;
#6479 = AXIS2_PLACEMENT_3D ( 'NONE', #739, #15989, #20363 ) ;
#6480 = B_SPLINE_CURVE_WITH_KNOTS ( 'NONE', 3,
 ( #6349, #23458, #6482, #6626, #15117, #13246, #12690, #11126, #21320, #4086, #10568, #1960, #8457, #23865 ),
 .UNSPECIFIED., .F., .F.,
 ( 4, 2, 2, 2, 2, 2, 4 ),
 ( -0.006894311516889582540, -0.006402023259230029545, -0.005909735001570475682, -0.004925158486251331527, -0.003940581970932187372, -0.003448293713272615295, -0.002956005455613042350 ),
 .UNSPECIFIED. ) ;
#6481 = CARTESIAN_POINT ( 'NONE',  ( 0.000000000000000000, 0.000000000000000000, -4.097771653543307347E-17 ) ) ;
#6482 = CARTESIAN_POINT ( 'NONE',  ( -0.09777734206179262977, 0.2994020000292518247, -3.561217286890655309 ) ) ;
#6483 = CARTESIAN_POINT ( 'NONE',  ( 0.4126915023378835423, -0.2375990494930988739, 0.2330651857771384172 ) ) ;
#6484 = ORIENTED_EDGE ( 'NONE', *, *, #24237, .T. ) ;
#6485 = TOROIDAL_SURFACE ( 'NONE', #21367, 0.6102362204724409711, 0.1299212598425196763 ) ;
#6487 = ADVANCED_FACE ( 'NONE', ( #7002 ), #8554, .T. ) ;
#6486 = CIRCLE ( 'NONE', #26330, 1.288838582677166222 ) ;
#6488 = CARTESIAN_POINT ( 'NONE',  ( -0.07874015748031495954, -1.062017969535966354E-23, -0.4653543306978102367 ) ) ;
#6489 = AXIS2_PLACEMENT_3D ( 'NONE', #15563, #6520, #15152 ) ;
#6490 = CARTESIAN_POINT ( 'NONE',  ( 0.0004405150045524555734, 0.6212597256746514862, 0.2574819594177531479 ) ) ;
#6491 = EDGE_CURVE ( 'NONE', #6015, #5312, #26470, .T. ) ;
#6492 = CARTESIAN_POINT ( 'NONE',  ( -0.0006362927944362226432, 0.4836123550485326716, 0.2715646632801987925 ) ) ;
#6493 = EDGE_CURVE ( 'NONE', #27472, #5887, #19718, .T. ) ;
#6494 = CARTESIAN_POINT ( 'NONE',  ( -0.2647715730835492609, -0.5498038367121063086, 0.2362204724409449064 ) ) ;
#6495 = CARTESIAN_POINT ( 'NONE',  ( 0.3214446924536846772, 0.3840069416942866742, 0.09685039370078740717 ) ) ;
#6496 = DIRECTION ( 'NONE',  ( 0.000000000000000000, 7.180547322999998243E-06, 0.9999999999742198442 ) ) ;
#6497 = CARTESIAN_POINT ( 'NONE',  ( -0.02576258753919771077, 0.1968503937007873850, -3.176774343053085481 ) ) ;
#6498 = ORIENTED_EDGE ( 'NONE', *, *, #11729, .F. ) ;
#6499 = ORIENTED_EDGE ( 'NONE', *, *, #21788, .F. ) ;
#6500 = LINE ( 'NONE', #27562, #14787 ) ;
#6501 = FACE_OUTER_BOUND ( 'NONE', #996, .T. ) ;
#6502 = EDGE_LOOP ( 'NONE', ( #1870, #22867 ) ) ;
#6503 = AXIS2_PLACEMENT_3D ( 'NONE', #8376, #23771, #8641 ) ;
#6504 = FACE_OUTER_BOUND ( 'NONE', #5555, .T. ) ;
#6505 = DIRECTION ( 'NONE',  ( 0.000000000000000000, 0.000000000000000000, -1.000000000000000000 ) ) ;
#6506 = AXIS2_PLACEMENT_3D ( 'NONE', #3472, #9981, #1509 ) ;
#6507 = ORIENTED_EDGE ( 'NONE', *, *, #8834, .F. ) ;
#6508 = CARTESIAN_POINT ( 'NONE',  ( -0.5335524835332036142, 0.1429116519061177371, 0.9399606299212598381 ) ) ;
#6509 = CARTESIAN_POINT ( 'NONE',  ( 0.3785000865565943395, 0.3010298976875371291, 0.2715646632839407437 ) ) ;
#6510 = ORIENTED_EDGE ( 'NONE', *, *, #8464, .T. ) ;
#6511 = CARTESIAN_POINT ( 'NONE',  ( 0.000000000000000000, 0.000000000000000000, -0.2755905511811023723 ) ) ;
#6512 = DIRECTION ( 'NONE',  ( -0.2588190448135648802, 3.169619147893076053E-17, 0.9659258263664937116 ) ) ;
#6513 = CARTESIAN_POINT ( 'NONE',  ( 0.3122922550372661532, 0.3730863453251304085, 0.2467937633102478545 ) ) ;
#6514 = CARTESIAN_POINT ( 'NONE',  ( 0.03008364706454716778, -0.2273032555864669124, 2.185478346456692557E-17 ) ) ;
#6515 = CARTESIAN_POINT ( 'NONE',  ( -0.3122765577857348207, -0.4068916527365984415, -1.550196850393700476 ) ) ;
#6516 = DIRECTION ( 'NONE',  ( 0.000000000000000000, 0.000000000000000000, -1.000000000000000000 ) ) ;
#6517 = AXIS2_PLACEMENT_3D ( 'NONE', #23769, #15021, #2411 ) ;
#6518 = CARTESIAN_POINT ( 'NONE',  ( 0.07874015748031489015, 0.1968503937007874127, -3.272637795275590733 ) ) ;
#6519 = DIRECTION ( 'NONE',  ( 1.000000000000000000, 0.000000000000000000, 0.000000000000000000 ) ) ;
#6520 = DIRECTION ( 'NONE',  ( 0.000000000000000000, 0.000000000000000000, -1.000000000000000000 ) ) ;
#6521 = ADVANCED_FACE ( 'NONE', ( #8833 ), #25698, .F. ) ;
#6522 = DIRECTION ( 'NONE',  ( -1.000000000000000000, 0.000000000000000000, 0.000000000000000000 ) ) ;
#6523 = DIRECTION ( 'NONE',  ( 0.000000000000000000, 0.000000000000000000, -1.000000000000000000 ) ) ;
#6524 = DIRECTION ( 'NONE',  ( 0.4338837391175580094, -0.9009688679024192570, 0.000000000000000000 ) ) ;
#6525 = CIRCLE ( 'NONE', #19618, 0.6299212598425196763 ) ;
#6526 = CARTESIAN_POINT ( 'NONE',  ( 0.2529800193559378352, 0.5131133041953702678, 0.9399606299212598381 ) ) ;
#6527 = CARTESIAN_POINT ( 'NONE',  ( -0.03359157810863924731, -0.5118096047256377457, -1.550196850393700920 ) ) ;
#6528 = AXIS2_PLACEMENT_3D ( 'NONE', #21597, #6077, #16662 ) ;
#6529 = CARTESIAN_POINT ( 'NONE',  ( 0.6117062799105453808, 0.1085321106658576895, 0.09685039370078740717 ) ) ;
#6530 = ORIENTED_EDGE ( 'NONE', *, *, #2877, .T. ) ;
#6531 = DIRECTION ( 'NONE',  ( -0.000000000000000000, -1.000000000000000000, -0.000000000000000000 ) ) ;
#6532 = ORIENTED_EDGE ( 'NONE', *, *, #24900, .T. ) ;
#6533 = AXIS2_PLACEMENT_3D ( 'NONE', #43, #8605, #24534 ) ;
#6534 = ORIENTED_EDGE ( 'NONE', *, *, #26548, .F. ) ;
#6535 = CARTESIAN_POINT ( 'NONE',  ( 0.4600326175569787179, -0.2268096725200276775, -1.550196850393700920 ) ) ;
#6536 = CARTESIAN_POINT ( 'NONE',  ( 0.5708661417322835607, 6.829619984160658046E-17, 0.9399606299212598381 ) ) ;
#6537 = DIRECTION ( 'NONE',  ( 0.000000000000000000, 1.000000000000000000, 0.000000000000000000 ) ) ;
#6538 = EDGE_CURVE ( 'NONE', #5084, #11259, #25716, .T. ) ;
#6539 = EDGE_LOOP ( 'NONE', ( #14520, #16363 ) ) ;
#6540 = B_SPLINE_CURVE_WITH_KNOTS ( 'NONE', 3,
 ( #22455, #17908, #7342, #3082, #22040, #11715, #26977, #26830, #7480, #7628 ),
 .UNSPECIFIED., .F., .F.,
 ( 4, 2, 2, 2, 4 ),
 ( 0.000000000000000000, 0.2500000000000000000, 0.5000000000000000000, 0.7500000000000000000, 1.000000000000000000 ),
 .UNSPECIFIED. ) ;
#6541 = DIRECTION ( 'NONE',  ( 1.000000000000000000, 0.000000000000000000, 0.000000000000000000 ) ) ;
#6542 = VERTEX_POINT ( 'NONE', #4464 ) ;
#6543 = AXIS2_PLACEMENT_3D ( 'NONE', #27100, #14253, #16635 ) ;
#6544 = DIRECTION ( 'NONE',  ( 0.2036417511401769909, 0.4895227362422910344, -0.8478782506317890100 ) ) ;
#6545 = PRODUCT_DEFINITION ( 'UNKNOWN', '', #14348, #23796 ) ;
#6546 = AXIS2_PLACEMENT_3D ( 'NONE', #25374, #1781, #23557 ) ;
#6547 = CARTESIAN_POINT ( 'NONE',  ( -0.6119360453657125554, 0.1072290460171901605, 0.09685039370078740717 ) ) ;
#6548 = FACE_OUTER_BOUND ( 'NONE', #16522, .T. ) ;
#6549 = ADVANCED_FACE ( 'NONE', ( #22241 ), #11271, .F. ) ;
#6550 = CARTESIAN_POINT ( 'NONE',  ( -0.4339912984563299436, -0.2498791196563492356, 0.2574803149606298969 ) ) ;
#6551 = DIRECTION ( 'NONE',  ( -1.000000000000000000, 0.000000000000000000, 0.000000000000000000 ) ) ;
#6552 = ADVANCED_FACE ( 'NONE', ( #11507 ), #17126, .T. ) ;
#6553 = EDGE_CURVE ( 'NONE', #26847, #15456, #2471, .T. ) ;
#6554 = ORIENTED_EDGE ( 'NONE', *, *, #14242, .F. ) ;
#6555 = DIRECTION ( 'NONE',  ( 1.000000000000000000, 0.000000000000000000, 0.000000000000000000 ) ) ;
#6556 = DIRECTION ( 'NONE',  ( 0.000000000000000000, 0.000000000000000000, -1.000000000000000000 ) ) ;
#6557 = CARTESIAN_POINT ( 'NONE',  ( -0.06441834428466812479, 0.4889536969035060410, -1.550196850393700920 ) ) ;
#6558 = AXIS2_PLACEMENT_3D ( 'NONE', #3916, #8435, #21152 ) ;
#6559 = CARTESIAN_POINT ( 'NONE',  ( 0.4382752542995623779, 0.1173917140416305405, -1.934055118110236338 ) ) ;
#6560 = APPLICATION_CONTEXT ( 'automotive_design' ) ;
#6561 = VECTOR ( 'NONE', #26725, 39.37007874015748143 ) ;
#6562 = CARTESIAN_POINT ( 'NONE',  ( 0.3606190329934327310, 0.4297690281277732338, 0.1771653543307086520 ) ) ;
#6563 = VERTEX_POINT ( 'NONE', #20121 ) ;
#6564 = CIRCLE ( 'NONE', #3854, 0.3464566929133857665 ) ;
#6565 = CARTESIAN_POINT ( 'NONE',  ( -0.6562077975700453258, 2.612916929133858441E-14, 0.2362204724409449064 ) ) ;
#6566 = SURFACE_STYLE_FILL_AREA ( #2447 ) ;
#6567 = CARTESIAN_POINT ( 'NONE',  ( -0.2355331214654103611, -0.4777261797697372470, 1.747047244094488194 ) ) ;
#6568 = DIRECTION ( 'NONE',  ( 0.000000000000000000, 0.000000000000000000, -1.000000000000000000 ) ) ;
#6569 = ORIENTED_EDGE ( 'NONE', *, *, #2848, .F. ) ;
#6570 = CARTESIAN_POINT ( 'NONE',  ( -0.6707652279343347956, -0.1538768215240151616, 0.3401574803149606252 ) ) ;
#6571 = CARTESIAN_POINT ( 'NONE',  ( 0.2131049448083992270, -0.5835666837866889667, 0.09685039370078740717 ) ) ;
#6572 = AXIS2_PLACEMENT_3D ( 'NONE', #9486, #7674, #14179 ) ;
#6573 = CARTESIAN_POINT ( 'NONE',  ( -0.6587140840999922142, 0.007992779901115512273, 0.07874015870966120934 ) ) ;
#6574 = VERTEX_POINT ( 'NONE', #8967 ) ;
#6575 = ADVANCED_FACE ( 'NONE', ( #11096 ), #782, .F. ) ;
#6576 = DIRECTION ( 'NONE',  ( 1.000000000000000000, 0.000000000000000000, 0.000000000000000000 ) ) ;
#6577 = CARTESIAN_POINT ( 'NONE',  ( 0.5190368482393039606, -0.1180105360553401483, 0.1322818204150990051 ) ) ;
#6578 = CARTESIAN_POINT ( 'NONE',  ( -0.4126915023499354573, -0.2375990495000580294, 0.1212655228631613069 ) ) ;
#6579 = ADVANCED_FACE ( 'NONE', ( #9227 ), #2684, .F. ) ;
#6580 = CARTESIAN_POINT ( 'NONE',  ( 0.1520645003235147619, -0.2938566582844236441, -0.3972204521082409734 ) ) ;
#6581 = B_SPLINE_CURVE_WITH_KNOTS ( 'NONE', 3,
 ( #9700, #22277, #2910, #15923, #11542, #18299, #20157, #11968, #816, #5613, #9404, #22848, #26944, #3474, #3326, #12102, #24528, #2033 ),
 .UNSPECIFIED., .F., .F.,
 ( 4, 2, 2, 2, 2, 2, 2, 2, 4 ),
 ( 0.5000000000000000000, 0.5625000000000000000, 0.6250000000000000000, 0.6875000000000000000, 0.7500000000000000000, 0.8125000000000000000, 0.8750000000000001110, 0.9375000000000001110, 1.000000000000000000 ),
 .UNSPECIFIED. ) ;
#6582 = FACE_OUTER_BOUND ( 'NONE', #22443, .T. ) ;
#6583 = EDGE_CURVE ( 'NONE', #25216, #7273, #13982, .T. ) ;
#6584 = CARTESIAN_POINT ( 'NONE',  ( -0.2169784220102915218, -0.4520537072505400045, 0.3080453759295606053 ) ) ;
#6585 = CARTESIAN_POINT ( 'NONE',  ( 0.2807137536170455361, -0.2462256503455606815, -3.115157480314960647 ) ) ;
#6586 = EDGE_CURVE ( 'NONE', #833, #15551, #2119, .T. ) ;
#6587 = VECTOR ( 'NONE', #22593, 39.37007874015748143 ) ;
#6588 = CARTESIAN_POINT ( 'NONE',  ( -0.09842519685039387289, 0.2165354330708660902, -3.561112174596415159 ) ) ;
#6589 = PRESENTATION_STYLE_ASSIGNMENT (( #21553 ) ) ;
#6590 = CARTESIAN_POINT ( 'NONE',  ( 0.5610236220472440971, 0.000000000000000000, 0.1771653543307086520 ) ) ;
#6591 = VERTEX_POINT ( 'NONE', #1652 ) ;
#6592 = CARTESIAN_POINT ( 'NONE',  ( -0.6117062799105531523, 0.1085321106658068829, 0.2574803149606298969 ) ) ;
#6593 = AXIS2_PLACEMENT_3D ( 'NONE', #14220, #18421, #24929 ) ;
#6594 = VERTEX_POINT ( 'NONE', #9706 ) ;
#6595 = DIRECTION ( 'NONE',  ( 1.000000000000000000, 0.000000000000000000, 0.000000000000000000 ) ) ;
#6596 = VERTEX_POINT ( 'NONE', #25101 ) ;
#6597 = CARTESIAN_POINT ( 'NONE',  ( 0.3432721300525757857, 0.06002180498097315492, 0.1166443193853626548 ) ) ;
#6598 = CARTESIAN_POINT ( 'NONE',  ( 0.1522836969815822838, 0.1970374587168192970, 0.4531137400420984229 ) ) ;
#6599 = APPLICATION_PROTOCOL_DEFINITION ( 'draft international standard', 'automotive_design', 1998, #11249 ) ;
#6600 = CARTESIAN_POINT ( 'NONE',  ( 0.3121994997598427912, 0.4069448477556012467, 1.766732283464566899 ) ) ;
#6601 = CARTESIAN_POINT ( 'NONE',  ( -0.4856708409200505283, -0.1649135259617098836, 1.747047244094488194 ) ) ;
#6602 = CARTESIAN_POINT ( 'NONE',  ( 0.000000000000000000, 0.000000000000000000, 0.1771653543307086520 ) ) ;
#6603 = VERTEX_POINT ( 'NONE', #9988 ) ;
#6604 = EDGE_LOOP ( 'NONE', ( #15331, #13608 ) ) ;
#6605 = CARTESIAN_POINT ( 'NONE',  ( -0.3233561589688984661, 0.1867299569291787087, -3.115157480314960647 ) ) ;
#6606 = EDGE_LOOP ( 'NONE', ( #3664, #15676, #23156, #25583, #4104 ) ) ;
#6607 = CIRCLE ( 'NONE', #727, 0.05216535433070866590 ) ;
#6608 = ORIENTED_EDGE ( 'NONE', *, *, #8944, .F. ) ;
#6609 = DIRECTION ( 'NONE',  ( -0.7660444431189780135, -0.6427876096865392519, 0.000000000000000000 ) ) ;
#6610 = SHAPE_REPRESENTATION_RELATIONSHIP ( 'NONE' , 'NONE' ,  #22737, #5624 ) ;
#6611 = FACE_OUTER_BOUND ( 'NONE', #6786, .T. ) ;
#6612 = CARTESIAN_POINT ( 'NONE',  ( -0.3007905576423956506, 0.1482986320106521871, 1.953740157480315043 ) ) ;
#6613 = ORIENTED_EDGE ( 'NONE', *, *, #9048, .F. ) ;
#6614 = VERTEX_POINT ( 'NONE', #14388 ) ;
#6615 = EDGE_CURVE ( 'NONE', #11455, #6009, #5831, .T. ) ;
#6616 = CIRCLE ( 'NONE', #21494, 0.7874015748208159637 ) ;
#6617 = ( BOUNDED_CURVE ( )  B_SPLINE_CURVE ( 3, ( #20818, #21632, #27326, #3721 ),
 .UNSPECIFIED., .F., .F. ) 
 B_SPLINE_CURVE_WITH_KNOTS ( ( 4, 4 ),
 ( 0.000000000000000000, 0.1131662519098511482 ),
 .UNSPECIFIED. ) 
 CURVE ( )  GEOMETRIC_REPRESENTATION_ITEM ( )  RATIONAL_B_SPLINE_CURVE ( ( 1.000000000000000000, 0.9989330679932157953, 0.9989330679932157953, 1.000000000000000000 ) ) 
 REPRESENTATION_ITEM ( '' )  ) ;
#6618 = LINE ( 'NONE', #26362, #2826 ) ;
#6619 = ORIENTED_EDGE ( 'NONE', *, *, #1343, .T. ) ;
#6620 = ORIENTED_EDGE ( 'NONE', *, *, #16004, .T. ) ;
#6621 = VERTEX_POINT ( 'NONE', #18738 ) ;
#6622 = LINE ( 'NONE', #4222, #7707 ) ;
#6623 = EDGE_CURVE ( 'NONE', #22088, #16756, #3566, .T. ) ;
#6624 = CONTEXT_DEPENDENT_SHAPE_REPRESENTATION ( #20071, #7585 ) ;
#6625 = CARTESIAN_POINT ( 'NONE',  ( 0.4563908000639795848, 0.8133290948875807613, -0.5151991767489622065 ) ) ;
#6626 = CARTESIAN_POINT ( 'NONE',  ( -0.09524605906741696881, 0.3002168457537168766, -3.573866392918775503 ) ) ;
#6627 = CARTESIAN_POINT ( 'NONE',  ( 0.7266071376980735019, 0.7048822860824826009, 0.02652157274389425196 ) ) ;
#6628 = ORIENTED_EDGE ( 'NONE', *, *, #5694, .T. ) ;
#6629 = ADVANCED_FACE ( 'NONE', ( #27518 ), #24064, .F. ) ;
#6630 = VERTEX_POINT ( 'NONE', #3518 ) ;
#6631 = EDGE_CURVE ( 'NONE', #7391, #27673, #25021, .T. ) ;
#6632 = FACE_OUTER_BOUND ( 'NONE', #20173, .T. ) ;
#6633 = VECTOR ( 'NONE', #14478, 39.37007874015748143 ) ;
#6634 = EDGE_CURVE ( 'NONE', #24688, #2747, #2234, .T. ) ;
#6635 = CARTESIAN_POINT ( 'NONE',  ( 0.07874015748031495954, 0.04546065111729338803, -0.4724409448818898127 ) ) ;
#6636 = CIRCLE ( 'NONE', #1661, 0.5511811023622047445 ) ;
#6637 = CARTESIAN_POINT ( 'NONE',  ( -4.821444091131312140E-17, -0.3937007874015748254, 0.01181102362204724393 ) ) ;
#6638 = CARTESIAN_POINT ( 'NONE',  ( -0.5189874374926378708, -0.1182276436463389618, 0.1322810039474935084 ) ) ;
#6639 = CARTESIAN_POINT ( 'NONE',  ( 1.197070535079588716, 0.4724409448818898127, -1.197070535079588716 ) ) ;
#6640 = EDGE_LOOP ( 'NONE', ( #442, #16200 ) ) ;
#6641 = CARTESIAN_POINT ( 'NONE',  ( -0.8725268807032540153, 0.000000000000000000, -1.052618110236220428 ) ) ;
#6642 = SHAPE_REPRESENTATION_RELATIONSHIP ( 'NONE' , 'NONE' ,  #25798, #26182 ) ;
#6643 = EDGE_LOOP ( 'NONE', ( #22688, #22613, #16731, #9252 ) ) ;
#6644 = CARTESIAN_POINT ( 'NONE',  ( 0.000000000000000000, 0.000000000000000000, -3.278217716535432842E-17 ) ) ;
#6645 = EDGE_CURVE ( 'NONE', #19029, #17602, #17988, .T. ) ;
#6646 = CARTESIAN_POINT ( 'NONE',  ( 0.2249706821157846648, -0.8351807821610452987, -0.2761312587482271375 ) ) ;
#6647 = ORIENTED_EDGE ( 'NONE', *, *, #4744, .F. ) ;
#6648 = LINE ( 'NONE', #2660, #17868 ) ;
#6649 = CARTESIAN_POINT ( 'NONE',  ( -0.5736786984127190125, 1.107101695597654922, -0.07148403028362050604 ) ) ;
#6650 = CARTESIAN_POINT ( 'NONE',  ( -0.3785000865568526884, 0.3010298976877424648, 0.2008762815967665150 ) ) ;
#6651 = ORIENTED_EDGE ( 'NONE', *, *, #3902, .F. ) ;
#6652 = CARTESIAN_POINT ( 'NONE',  ( -0.3362148458988027944, 0.4382482975805537806, 0.9399606299212598381 ) ) ;
#6653 = EDGE_LOOP ( 'NONE', ( #3461, #12252 ) ) ;
#6654 = DIRECTION ( 'NONE',  ( 0.000000000000000000, -1.000000000000000000, 0.000000000000000000 ) ) ;
#6655 = EDGE_CURVE ( 'NONE', #5423, #1388, #10930, .T. ) ;
#6656 = CARTESIAN_POINT ( 'NONE',  ( 0.6614173228346456046, 8.100026073100603114E-17, -0.01377952755905511792 ) ) ;
#6657 = VERTEX_POINT ( 'NONE', #9593 ) ;
#6658 = CARTESIAN_POINT ( 'NONE',  ( -0.0007595033562148819414, 0.6881885572739390167, 0.3401574803149606252 ) ) ;
#6659 = AXIS2_PLACEMENT_3D ( 'NONE', #3164, #7146, #24640 ) ;
#6660 = CARTESIAN_POINT ( 'NONE',  ( 0.3905379133858267737, -0.5610236220472440971, 6.870559055118111198E-17 ) ) ;
#6661 = CARTESIAN_POINT ( 'NONE',  ( -0.1771653543307086520, -0.8267716535433071723, 1.012503259137575512E-16 ) ) ;
#6662 = DIRECTION ( 'NONE',  ( -0.9790454724845842893, 0.2036417511401760472, 0.000000000000000000 ) ) ;
#6663 = CARTESIAN_POINT ( 'NONE',  ( -0.2420394123212937232, 0.2892587550802429575, 0.07637795275590551769 ) ) ;
#6664 = DIRECTION ( 'NONE',  ( 0.000000000000000000, 0.000000000000000000, 1.000000000000000000 ) ) ;
#6665 = DIRECTION ( 'NONE',  ( -0.2036417511401760472, 0.4895227362422920336, 0.8478782506317883438 ) ) ;
#6666 = CARTESIAN_POINT ( 'NONE',  ( -1.456051859514965975E-17, 0.4692913385826771866, 0.1992150590373740204 ) ) ;
#6667 = CARTESIAN_POINT ( 'NONE',  ( -0.1968503937007874127, -5.733057234251967840E-18, -0.1476377952755905387 ) ) ;
#6668 = CARTESIAN_POINT ( 'NONE',  ( -0.3200513472080661614, 0.3804946224892518103, 0.1140743250936718939 ) ) ;
#6669 = CARTESIAN_POINT ( 'NONE',  ( 0.2529800193559499921, -0.5131133041954075713, 0.9399606299212598381 ) ) ;
#6670 = AXIS2_PLACEMENT_3D ( 'NONE', #21700, #1924, #6313 ) ;
#6671 = FACE_OUTER_BOUND ( 'NONE', #21866, .T. ) ;
#6672 = ORIENTED_EDGE ( 'NONE', *, *, #14295, .T. ) ;
#6673 = CARTESIAN_POINT ( 'NONE',  ( 0.000000000000000000, 0.07874015748031491790, -1.692913385826771533 ) ) ;
#6674 = CIRCLE ( 'NONE', #22447, 0.1298643763538142593 ) ;
#6675 = ORIENTED_EDGE ( 'NONE', *, *, #27515, .T. ) ;
#6676 = ORIENTED_EDGE ( 'NONE', *, *, #17110, .T. ) ;
#6677 = CARTESIAN_POINT ( 'NONE',  ( -0.09139240964747707974, -0.07874015748031501505, -0.02109836160874977232 ) ) ;
#6678 = CARTESIAN_POINT ( 'NONE',  ( 0.000000000000000000, -0.09092130223458683158, -0.3779527559055118058 ) ) ;
#6679 = VERTEX_POINT ( 'NONE', #26416 ) ;
#6680 = EDGE_CURVE ( 'NONE', #17014, #11142, #12214, .T. ) ;
#6681 = CARTESIAN_POINT ( 'NONE',  ( -0.2243804351500972571, 0.2666304421183634532, 0.1589462317874973663 ) ) ;
#6682 = ORIENTED_EDGE ( 'NONE', *, *, #12822, .T. ) ;
#6683 = AXIS2_PLACEMENT_3D ( 'NONE', #8488, #27854, #17112 ) ;
#6684 = VECTOR ( 'NONE', #27612, 39.37007874015748854 ) ;
#6685 = CARTESIAN_POINT ( 'NONE',  ( -0.6117062799105453808, 0.1085321106658580781, 0.09685039370078740717 ) ) ;
#6686 = DIRECTION ( 'NONE',  ( -0.4999999999999996114, -0.8660254037844389297, 0.000000000000000000 ) ) ;
#6687 = DIRECTION ( 'NONE',  ( 0.000000000000000000, 0.000000000000000000, -1.000000000000000000 ) ) ;
#6688 = FACE_OUTER_BOUND ( 'NONE', #17979, .T. ) ;
#6689 = CARTESIAN_POINT ( 'NONE',  ( -0.2078289949484350141, -0.4330237525397957477, 0.2362204724409447676 ) ) ;
#6690 = ORIENTED_EDGE ( 'NONE', *, *, #8529, .T. ) ;
#6691 = CARTESIAN_POINT ( 'NONE',  ( -0.4327133464943124785, -0.2505177833310021085, 0.1496602734626562570 ) ) ;
#6692 = CARTESIAN_POINT ( 'NONE',  ( -0.09842519685039370636, -0.07874015748031495954, -0.04546065111729338803 ) ) ;
#6693 = B_SPLINE_CURVE_WITH_KNOTS ( 'NONE', 3,
 ( #5659, #18341, #20628, #14136, #24708, #14283 ),
 .UNSPECIFIED., .F., .F.,
 ( 4, 2, 4 ),
 ( 0.000000000000000000, 0.2500000000000000000, 0.5000000000000000000 ),
 .UNSPECIFIED. ) ;
#6694 = CARTESIAN_POINT ( 'NONE',  ( 0.3001918266902269261, 0.3912931228431901776, -1.550196850393700920 ) ) ;
#6695 = CARTESIAN_POINT ( 'NONE',  ( -0.06001958459474868862, 0.4555658499976078524, -1.928289503579158515 ) ) ;
#6696 = CARTESIAN_POINT ( 'NONE',  ( -0.6003937007829848183, 1.122047244090071727, 1.315345636034250449E-15 ) ) ;
#6697 = DIRECTION ( 'NONE',  ( 1.000000000000000000, 0.000000000000000000, 0.000000000000000000 ) ) ;
#6698 = AXIS2_PLACEMENT_3D ( 'NONE', #2766, #5172, #4758 ) ;
#6699 = EDGE_CURVE ( 'NONE', #2591, #19036, #24790, .T. ) ;
#6700 = CARTESIAN_POINT ( 'NONE',  ( 0.1610509776512037416, -0.4407912692718771175, 0.07637795275590551769 ) ) ;
#6701 = AXIS2_PLACEMENT_3D ( 'NONE', #26793, #26647, #13658 ) ;
#6702 = AXIS2_PLACEMENT_3D ( 'NONE', #27359, #27504, #16611 ) ;
#6703 = CIRCLE ( 'NONE', #5804, 0.3163739521363750362 ) ;
#6704 = CARTESIAN_POINT ( 'NONE',  ( 5.827097576719993621E-17, 0.6881889763779529545, 0.3401599409343964431 ) ) ;
#6705 = FACE_OUTER_BOUND ( 'NONE', #16059, .T. ) ;
#6706 = LINE ( 'NONE', #6292, #13874 ) ;
#6707 = ORIENTED_EDGE ( 'NONE', *, *, #23893, .F. ) ;
#6708 = DIRECTION ( 'NONE',  ( 1.000000000000000000, 0.000000000000000000, 0.000000000000000000 ) ) ;
#6709 = EDGE_CURVE ( 'NONE', #8713, #16564, #12628, .T. ) ;
#6710 = CARTESIAN_POINT ( 'NONE',  ( -0.4055118110236220486, -0.4724409448818898127, 0.8182917201112794858 ) ) ;
#6711 = VERTEX_POINT ( 'NONE', #5356 ) ;
#6712 = DIRECTION ( 'NONE',  ( 0.000000000000000000, 0.000000000000000000, 1.000000000000000000 ) ) ;
#6713 = ORIENTED_EDGE ( 'NONE', *, *, #22297, .F. ) ;
#6714 = CARTESIAN_POINT ( 'NONE',  ( -0.6912180915490531152, 0.1281909420063060967, 0.2299950541617507838 ) ) ;
#6715 = ORIENTED_EDGE ( 'NONE', *, *, #12974, .F. ) ;
#6716 = CARTESIAN_POINT ( 'NONE',  ( -0.4069519308876554664, 0.2006393256663590030, -1.934055118110236338 ) ) ;
#6717 = CARTESIAN_POINT ( 'NONE',  ( -0.1771653543307086520, 0.7903543307086614567, 0.000000000000000000 ) ) ;
#6718 = DIRECTION ( 'NONE',  ( 1.000000000000000000, 0.000000000000000000, 0.000000000000000000 ) ) ;
#6719 = DIRECTION ( 'NONE',  ( 0.000000000000000000, 0.000000000000000000, 1.000000000000000000 ) ) ;
#6720 = CARTESIAN_POINT ( 'NONE',  ( 0.2249706821157846648, -0.7189271281445788198, -0.3842149643474468412 ) ) ;
#6721 = DIRECTION ( 'NONE',  ( 1.000000000000000000, 0.000000000000000000, 0.000000000000000000 ) ) ;
#6722 = CIRCLE ( 'NONE', #16664, 0.7874015748031496509 ) ;
#6723 = AXIS2_PLACEMENT_3D ( 'NONE', #14094, #5770, #14250 ) ;
#6724 = CARTESIAN_POINT ( 'NONE',  ( 0.000000000000000000, 0.000000000000000000, -0.4724409448818898127 ) ) ;
#6725 = CARTESIAN_POINT ( 'NONE',  ( -0.3606853515406169275, 0.09660931395005029065, -3.115157480314960647 ) ) ;
#6726 = AXIS2_PLACEMENT_3D ( 'NONE', #9448, #20346, #20483 ) ;
#6727 = CARTESIAN_POINT ( 'NONE',  ( 0.03937007874015749365, -0.06819097667593998491, -0.3779527559055118058 ) ) ;
#6728 = CARTESIAN_POINT ( 'NONE',  ( -0.2358179517434294548, 0.2802411498267050605, 0.08455817588214351033 ) ) ;
#6729 = DIRECTION ( 'NONE',  ( 1.000000000000000000, 0.000000000000000000, 0.000000000000000000 ) ) ;
#6730 = ORIENTED_EDGE ( 'NONE', *, *, #20658, .T. ) ;
#6731 = CARTESIAN_POINT ( 'NONE',  ( 0.000000000000000000, 0.000000000000000000, 0.000000000000000000 ) ) ;
#6732 = EDGE_CURVE ( 'NONE', #19560, #18356, #760, .T. ) ;
#6733 = AXIS2_PLACEMENT_3D ( 'NONE', #20426, #22686, #9024 ) ;
#6734 = ADVANCED_FACE ( 'NONE', ( #9730 ), #9574, .T. ) ;
#6735 = ORIENTED_EDGE ( 'NONE', *, *, #9476, .T. ) ;
#6736 = EDGE_CURVE ( 'NONE', #21585, #10762, #19856, .T. ) ;
#6737 = DIRECTION ( 'NONE',  ( 1.000000000000000000, 0.000000000000000000, 0.000000000000000000 ) ) ;
#6738 = CARTESIAN_POINT ( 'NONE',  ( 0.4984899526255159308, 0.1339654526248287292, 1.766732283464566677 ) ) ;
#6739 = APPLICATION_PROTOCOL_DEFINITION ( 'draft international standard', 'automotive_design', 1998, #614 ) ;
#6740 = DIMENSIONAL_EXPONENTS ( 1.000000000000000000, 0.000000000000000000, 0.000000000000000000, 0.000000000000000000, 0.000000000000000000, 0.000000000000000000, 0.000000000000000000 ) ;
#6741 = FACE_OUTER_BOUND ( 'NONE', #22510, .T. ) ;
#6742 = EDGE_CURVE ( 'NONE', #21566, #19740, #22323, .T. ) ;
#6743 = CARTESIAN_POINT ( 'NONE',  ( -0.4856708409200499732, 0.1649135259616961724, 1.747047244094488194 ) ) ;
#6744 = DIRECTION ( 'NONE',  ( 0.000000000000000000, 1.000000000000000000, 0.000000000000000000 ) ) ;
#6745 = EDGE_LOOP ( 'NONE', ( #2551, #11655, #26223, #1573, #16919 ) ) ;
#6746 = ORIENTED_EDGE ( 'NONE', *, *, #22676, .F. ) ;
#6747 = AXIS2_PLACEMENT_3D ( 'NONE', #5943, #7635, #27131 ) ;
#6748 = CARTESIAN_POINT ( 'NONE',  ( -0.09660931395005634137, -0.3606853515406420185, -3.115157480314960647 ) ) ;
#6749 = EDGE_CURVE ( 'NONE', #11924, #14095, #11728, .T. ) ;
#6750 = ORIENTED_EDGE ( 'NONE', *, *, #19074, .T. ) ;
#6751 = DIRECTION ( 'NONE',  ( 0.2036417511401759084, -0.4895227362422918116, -0.8478782506317885659 ) ) ;
#6752 = CARTESIAN_POINT ( 'NONE',  ( 0.1504127680536208045, 0.2746298698235986602, -0.3999947715762637301 ) ) ;
#6753 = CARTESIAN_POINT ( 'NONE',  ( -0.1482986320106466638, 0.3007905576423924310, 1.953740157480315043 ) ) ;
#6754 = ORIENTED_EDGE ( 'NONE', *, *, #21479, .T. ) ;
#6755 = ORIENTED_EDGE ( 'NONE', *, *, #3958, .F. ) ;
#6756 = ORIENTED_EDGE ( 'NONE', *, *, #20212, .T. ) ;
#6757 = LINE ( 'NONE', #19739, #18628 ) ;
#6758 = EDGE_LOOP ( 'NONE', ( #7160, #14997 ) ) ;
#6759 = EDGE_LOOP ( 'NONE', ( #3804, #5642, #27625, #6952, #20686 ) ) ;
#6760 = ORIENTED_EDGE ( 'NONE', *, *, #27826, .F. ) ;
#6761 = CARTESIAN_POINT ( 'NONE',  ( 0.2083728861314909642, 0.3778799683988480762, -0.2992345713061846935 ) ) ;
#6762 = CARTESIAN_POINT ( 'NONE',  ( 8.741913385826771462E-17, 0.1328740157480315098, 0.000000000000000000 ) ) ;
#6763 = DIRECTION ( 'NONE',  ( 0.000000000000000000, 0.000000000000000000, -1.000000000000000000 ) ) ;
#6764 = CARTESIAN_POINT ( 'NONE',  ( 0.6343085930858298749, 0.8719994442144956004, -0.1034023825655943502 ) ) ;
#6765 = ORIENTED_EDGE ( 'NONE', *, *, #13241, .T. ) ;
#6766 = AXIS2_PLACEMENT_3D ( 'NONE', #7584, #14084, #22698 ) ;
#6767 = CARTESIAN_POINT ( 'NONE',  ( -1.452994488188976472E-16, 0.5905905511811023745, -3.646653543307086576 ) ) ;
#6768 = ( REPRESENTATION_RELATIONSHIP ('NONE','NONE', #12434, #27787 ) REPRESENTATION_RELATIONSHIP_WITH_TRANSFORMATION ( #987 )SHAPE_REPRESENTATION_RELATIONSHIP( ) ) ;
#6769 = CARTESIAN_POINT ( 'NONE',  ( -0.2128972891168661452, -0.5836425148029424914, 0.09684874924366436433 ) ) ;
#6770 = EDGE_CURVE ( 'NONE', #27702, #14224, #23023, .T. ) ;
#6771 = ORIENTED_EDGE ( 'NONE', *, *, #12058, .T. ) ;
#6772 = CARTESIAN_POINT ( 'NONE',  ( 0.000000000000000000, 0.000000000000000000, -0.04133858267716535029 ) ) ;
#6773 = DIRECTION ( 'NONE',  ( 0.000000000000000000, -1.000000000000000000, 0.000000000000000000 ) ) ;
#6774 = ADVANCED_FACE ( 'NONE', ( #20471 ), #16257, .F. ) ;
#6775 = CARTESIAN_POINT ( 'NONE',  ( 0.000000000000000000, 0.6881889763779527325, 0.06614173228346456601 ) ) ;
#6776 = DIRECTION ( 'NONE',  ( -0.3420201433256691570, -0.9396926207859082059, 0.000000000000000000 ) ) ;
#6777 = EDGE_LOOP ( 'NONE', ( #22873, #2494, #8661 ) ) ;
#6778 = DIRECTION ( 'NONE',  ( 0.000000000000000000, 1.000000000000000000, 0.000000000000000000 ) ) ;
#6779 = AXIS2_PLACEMENT_3D ( 'NONE', #9160, #22304, #11563 ) ;
#6780 = EDGE_LOOP ( 'NONE', ( #5061, #4071, #26309, #11047 ) ) ;
#6781 = FACE_OUTER_BOUND ( 'NONE', #9892, .T. ) ;
#6782 = CIRCLE ( 'NONE', #5879, 0.4980314960629921295 ) ;
#6783 = CARTESIAN_POINT ( 'NONE',  ( -0.1580799066051627177, -0.4326553680327468454, 0.1771653543307088186 ) ) ;
#6784 = CYLINDRICAL_SURFACE ( 'NONE', #9269, 0.1181102362204720091 ) ;
#6785 = CARTESIAN_POINT ( 'NONE',  ( 0.6299212598425196763, -1.895600393700787470E-35, 0.000000000000000000 ) ) ;
#6786 = EDGE_LOOP ( 'NONE', ( #24548, #7322, #27595, #18756 ) ) ;
#6787 = CARTESIAN_POINT ( 'NONE',  ( 0.5335524835332415838, 0.1429116519061139345, 0.9399606299212598381 ) ) ;
#6788 = B_SPLINE_CURVE_WITH_KNOTS ( 'NONE', 3,
 ( #21972, #6862, #23956, #24088 ),
 .UNSPECIFIED., .F., .F.,
 ( 4, 4 ),
 ( 0.4045103800602309896, 0.4064350009536160102 ),
 .UNSPECIFIED. ) ;
#6789 = DIRECTION ( 'NONE',  ( -1.000000000000000000, 0.000000000000000000, 0.000000000000000000 ) ) ;
#6790 = ORIENTED_EDGE ( 'NONE', *, *, #21213, .T. ) ;
#6791 = ( GEOMETRIC_REPRESENTATION_CONTEXT ( 3 ) GLOBAL_UNCERTAINTY_ASSIGNED_CONTEXT ( ( #3360 ) ) GLOBAL_UNIT_ASSIGNED_CONTEXT ( ( #12173, #16005, #5698 ) ) REPRESENTATION_CONTEXT ( 'NONE', 'WORKASPACE' ) ) ;
#6792 = DIRECTION ( 'NONE',  ( -1.000000000000000000, 0.000000000000000000, 0.000000000000000000 ) ) ;
#6793 = LINE ( 'NONE', #24156, #21283 ) ;
#6794 = DIRECTION ( 'NONE',  ( 0.000000000000000000, 1.000000000000000000, 0.000000000000000000 ) ) ;
#6795 = FACE_BOUND ( 'NONE', #27723, .T. ) ;
#6796 = ORIENTED_EDGE ( 'NONE', *, *, #11893, .T. ) ;
#6797 = DIRECTION ( 'NONE',  ( 0.000000000000000000, -1.000000000000000000, 0.000000000000000000 ) ) ;
#6798 = DIRECTION ( 'NONE',  ( -0.8660254037844390407, -0.4999999999999994449, 0.000000000000000000 ) ) ;
#6799 = CARTESIAN_POINT ( 'NONE',  ( -0.1771653543307086520, -5.663984251968503442E-18, 0.000000000000000000 ) ) ;
#6800 = CARTESIAN_POINT ( 'NONE',  ( -0.1968503937007874127, 0.000000000000000000, 0.000000000000000000 ) ) ;
#6801 = VERTEX_POINT ( 'NONE', #845 ) ;
#6802 = EDGE_CURVE ( 'NONE', #4649, #8161, #25738, .T. ) ;
#6803 = CIRCLE ( 'NONE', #1389, 2.066929133858267598 ) ;
#6804 = CARTESIAN_POINT ( 'NONE',  ( 0.3482225189666449672, 0.4539000224941344697, 0.9399606299212598381 ) ) ;
#6805 = EDGE_CURVE ( 'NONE', #12305, #4795, #15787, .T. ) ;
#6806 = DIRECTION ( 'NONE',  ( -0.000000000000000000, -1.000000000000000000, -0.000000000000000000 ) ) ;
#6807 = ORIENTED_EDGE ( 'NONE', *, *, #14443, .F. ) ;
#6808 = CARTESIAN_POINT ( 'NONE',  ( -0.5190862322091315262, -0.1177929122753175184, 0.3401574803149606252 ) ) ;
#6809 = EDGE_CURVE ( 'NONE', #14040, #13062, #15370, .T. ) ;
#6810 = ORIENTED_EDGE ( 'NONE', *, *, #24229, .T. ) ;
#6811 = VERTEX_POINT ( 'NONE', #26401 ) ;
#6812 = EDGE_CURVE ( 'NONE', #13503, #3374, #7195, .T. ) ;
#6813 = ORIENTED_EDGE ( 'NONE', *, *, #4157, .F. ) ;
#6814 = CARTESIAN_POINT ( 'NONE',  ( 0.03349795313024073878, -0.5118110236220473341, -1.550196850393700920 ) ) ;
#6815 = CARTESIAN_POINT ( 'NONE',  ( -2.185478346456693112E-16, 0.000000000000000000, 0.000000000000000000 ) ) ;
#6816 = CARTESIAN_POINT ( 'NONE',  ( 0.1294857240059045234, -0.3542416573274181357, 0.1992125984251968684 ) ) ;
#6817 = DIRECTION ( 'NONE',  ( 1.000000000000000000, 0.000000000000000000, 0.000000000000000000 ) ) ;
#6818 = CARTESIAN_POINT ( 'NONE',  ( 0.3528204557988524614, 0.06272520244146252699, 0.09506557083424545251 ) ) ;
#6819 = ORIENTED_EDGE ( 'NONE', *, *, #2646, .F. ) ;
#6820 = CARTESIAN_POINT ( 'NONE',  ( 0.000000000000000000, 0.000000000000000000, 0.2574803149606298969 ) ) ;
#6821 = ORIENTED_EDGE ( 'NONE', *, *, #10361, .T. ) ;
#6822 = EDGE_CURVE ( 'NONE', #25553, #20290, #18035, .T. ) ;
#6823 = LENGTH_MEASURE_WITH_UNIT ( LENGTH_MEASURE( 0.02539999999999999897 ), #23922 ) ;
#6824 = CIRCLE ( 'NONE', #3636, 0.8163976377952757435 ) ;
#6825 = CARTESIAN_POINT ( 'NONE',  ( -0.3338887748335582772, 0.000000000000000000, -1.052618110236220428 ) ) ;
#6826 = CARTESIAN_POINT ( 'NONE',  ( 0.000000000000000000, 0.000000000000000000, 0.2362204724409449064 ) ) ;
#6827 = ( NAMED_UNIT ( * ) PLANE_ANGLE_UNIT ( ) SI_UNIT ( $, .RADIAN. ) ) ;
#6828 = CARTESIAN_POINT ( 'NONE',  ( -0.2078289949484354027, -0.4330237525397954146, 0.2194422276617741807 ) ) ;
#6829 = ORIENTED_EDGE ( 'NONE', *, *, #20642, .T. ) ;
#6830 = CARTESIAN_POINT ( 'NONE',  ( -2.685748425196850164E-17, 0.000000000000000000, -1.934055118110236338 ) ) ;
#6831 = CARTESIAN_POINT ( 'NONE',  ( -0.03001016326913665336, -0.4585215200179055817, -1.928289503579156516 ) ) ;
#6832 = ORIENTED_EDGE ( 'NONE', *, *, #3694, .T. ) ;
#6833 = CARTESIAN_POINT ( 'NONE',  ( -0.5230301363771427958, 0.1775991818008358647, 0.9202755905511811330 ) ) ;
#6834 = LINE ( 'NONE', #24456, #23658 ) ;
#6835 = EDGE_CURVE ( 'NONE', #17724, #26290, #13546, .T. ) ;
#6836 = CARTESIAN_POINT ( 'NONE',  ( 0.2647715730835492609, -0.5498038367121063086, 0.3661437007874016047 ) ) ;
#6837 = DIRECTION ( 'NONE',  ( 0.000000000000000000, 0.000000000000000000, 1.000000000000000000 ) ) ;
#6838 = ADVANCED_FACE ( 'NONE', ( #5209, #24420 ), #5065, .T. ) ;
#6839 = AXIS2_PLACEMENT_3D ( 'NONE', #13373, #11526, #15909 ) ;
#6840 = EDGE_LOOP ( 'NONE', ( #19040, #9763, #16834, #9950 ) ) ;
#6841 = CARTESIAN_POINT ( 'NONE',  ( 0.000000000000000000, -0.09092130223458683158, -0.3779527559055118058 ) ) ;
#6842 = CARTESIAN_POINT ( 'NONE',  ( -0.5905511811023621549, -0.6348133144914153148, -0.8891632684400255782 ) ) ;
#6843 = DIRECTION ( 'NONE',  ( 1.000000000000000000, 0.000000000000000000, 0.000000000000000000 ) ) ;
#6844 = AXIS2_PLACEMENT_3D ( 'NONE', #15634, #7014, #398 ) ;
#6845 = MECHANICAL_DESIGN_GEOMETRIC_PRESENTATION_REPRESENTATION (  '', ( #6388 ), #8635 ) ;
#6846 = CARTESIAN_POINT ( 'NONE',  ( -0.07874015748031495954, 0.02307066120096010892, -0.4684762439721033012 ) ) ;
#6847 = DIRECTION ( 'NONE',  ( 1.000000000000000000, 0.000000000000000000, 0.000000000000000000 ) ) ;
#6848 = CARTESIAN_POINT ( 'NONE',  ( 0.3991696156513425686, 0.4760540497244023506, 0.2574827755769819038 ) ) ;
#6849 = CARTESIAN_POINT ( 'NONE',  ( 0.000000000000000000, 0.07874015746264864668, 0.000000000000000000 ) ) ;
#6850 = CARTESIAN_POINT ( 'NONE',  ( -0.7795729917428700917, 0.3433105971656929545, -0.1409633029682732241 ) ) ;
#6851 = ORIENTED_EDGE ( 'NONE', *, *, #4968, .F. ) ;
#6852 = CARTESIAN_POINT ( 'NONE',  ( -0.3996230174612653285, -0.1970259548082108347, -1.934055118110236338 ) ) ;
#6853 = DIRECTION ( 'NONE',  ( 0.9396926207859082059, 0.3420201433256690460, 0.000000000000000000 ) ) ;
#6854 = ORIENTED_EDGE ( 'NONE', *, *, #3309, .T. ) ;
#6855 = CARTESIAN_POINT ( 'NONE',  ( -0.3661417322834645272, -0.4724409448818898127, -0.9265594366467145848 ) ) ;
#6856 = CARTESIAN_POINT ( 'NONE',  ( 0.003937007874015826907, 7.887824528841537495E-18, 0.09842519685039370636 ) ) ;
#6857 = EDGE_CURVE ( 'NONE', #9819, #23096, #26713, .T. ) ;
#6858 = AXIS2_PLACEMENT_3D ( 'NONE', #18789, #20783, #1425 ) ;
#6859 = CARTESIAN_POINT ( 'NONE',  ( -0.2092582568878602056, -0.4359957531173518364, 0.2715646632357672785 ) ) ;
#6860 = CARTESIAN_POINT ( 'NONE',  ( -0.3572819248074391996, 0.1213180142433954029, -3.100567304031768057 ) ) ;
#6861 = DIRECTION ( 'NONE',  ( 1.000000000000000000, 0.000000000000000000, 0.000000000000000000 ) ) ;
#6862 = CARTESIAN_POINT ( 'NONE',  ( 0.0005057506112066535546, 0.6881888373222776467, 0.1322818203437346463 ) ) ;
#6863 = DIRECTION ( 'NONE',  ( 1.000000000000000000, 0.000000000000000000, 0.000000000000000000 ) ) ;
#6864 = ORIENTED_EDGE ( 'NONE', *, *, #8158, .F. ) ;
#6865 = CARTESIAN_POINT ( 'NONE',  ( 0.4811133747915324332, 5.891939544654311124E-17, -0.2755905511811023723 ) ) ;
#6866 = ORIENTED_EDGE ( 'NONE', *, *, #9739, .T. ) ;
#6867 = ORIENTED_EDGE ( 'NONE', *, *, #18492, .T. ) ;
#6868 = B_SPLINE_CURVE_WITH_KNOTS ( 'NONE', 3,
 ( #2444, #9075, #21810, #7842, #3569, #20550, #11641, #16447 ),
 .UNSPECIFIED., .F., .F.,
 ( 4, 2, 2, 4 ),
 ( 0.5000000000000000000, 0.7499999999999996669, 0.8749999999999997780, 1.000000000000000000 ),
 .UNSPECIFIED. ) ;
#6869 = CARTESIAN_POINT ( 'NONE',  ( 0.000000000000000000, 0.09092130223458683158, -0.3779527559055118058 ) ) ;
#6870 = CARTESIAN_POINT ( 'NONE',  ( 0.2577577458591218673, 0.4472135058506045424, 1.766732283464566899 ) ) ;
#6871 = CARTESIAN_POINT ( 'NONE',  ( -0.03937007874015754916, -0.06819097667594005430, -0.3779527559055118058 ) ) ;
#6872 = DIRECTION ( 'NONE',  ( 0.000000000000000000, 0.000000000000000000, -1.000000000000000000 ) ) ;
#6873 = CARTESIAN_POINT ( 'NONE',  ( -0.1327036767659477978, -0.4954415918530775120, 1.747047244094488194 ) ) ;
#6874 = CARTESIAN_POINT ( 'NONE',  ( -0.1771653543307086520, -5.663984251968503442E-18, -0.1476377952755905387 ) ) ;
#6875 = AXIS2_PLACEMENT_3D ( 'NONE', #23443, #10701, #15103 ) ;
#6876 = EDGE_LOOP ( 'NONE', ( #6058, #6672 ) ) ;
#6877 = AXIS2_PLACEMENT_3D ( 'NONE', #16800, #7907, #20474 ) ;
#6878 = ORIENTED_EDGE ( 'NONE', *, *, #1320, .T. ) ;
#6880 = CARTESIAN_POINT ( 'NONE',  ( 0.02438677169350735724, -0.3726024258163779246, -3.115157480314960647 ) ) ;
#6879 = CARTESIAN_POINT ( 'NONE',  ( 0.5510854067045450888, 0.4384931681290698546, 0.1443310008641096598 ) ) ;
#6881 = ORIENTED_EDGE ( 'NONE', *, *, #4467, .F. ) ;
#6882 = CARTESIAN_POINT ( 'NONE',  ( 0.000000000000000000, 0.000000000000000000, -0.04133858267716535029 ) ) ;
#6883 = LINE ( 'NONE', #11521, #4665 ) ;
#6884 = CARTESIAN_POINT ( 'NONE',  ( -0.3239425792934415571, -0.08676778863010886633, 1.953740157480315043 ) ) ;
#6885 = ORIENTED_EDGE ( 'NONE', *, *, #3641, .T. ) ;
#6886 = EDGE_LOOP ( 'NONE', ( #17915, #414, #18388, #8067, #26558 ) ) ;
#6887 = ORIENTED_EDGE ( 'NONE', *, *, #7653, .T. ) ;
#6888 = CIRCLE ( 'NONE', #27663, 0.4173606904906118076 ) ;
#6889 = CARTESIAN_POINT ( 'NONE',  ( 0.000000000000000000, 0.000000000000000000, 0.3401574803149606252 ) ) ;
#6890 = ORIENTED_EDGE ( 'NONE', *, *, #5230, .T. ) ;
#6891 = VERTEX_POINT ( 'NONE', #7767 ) ;
#6892 = ORIENTED_EDGE ( 'NONE', *, *, #24202, .T. ) ;
#6893 = FACE_OUTER_BOUND ( 'NONE', #12536, .T. ) ;
#6894 = EDGE_CURVE ( 'NONE', #1047, #1806, #21030, .T. ) ;
#6895 = LINE ( 'NONE', #15525, #20299 ) ;
#6896 = PRODUCT_DEFINITION ( 'UNKNOWN', '', #11565, #26900 ) ;
#6897 = CARTESIAN_POINT ( 'NONE',  ( -0.5511811023268710086, 0.000000000000000000, 1.747047244094488194 ) ) ;
#6898 = CARTESIAN_POINT ( 'NONE',  ( 0.5985371529601012375, 0.9200311766420431470, -0.1500396732972504588 ) ) ;
#6899 = PRODUCT_DEFINITION_SHAPE ( 'NONE', 'NONE',  #27906 ) ;
#6900 = ADVANCED_FACE ( 'NONE', ( #14565 ), #26601, .F. ) ;
#6901 = CIRCLE ( 'NONE', #19971, 0.3771653543307086909 ) ;
#6902 = CIRCLE ( 'NONE', #24475, 0.1318897637674579792 ) ;
#6903 = CARTESIAN_POINT ( 'NONE',  ( 0.000000000000000000, 0.000000000000000000, 0.09685039370078740717 ) ) ;
#6904 = AXIS2_PLACEMENT_3D ( 'NONE', #26516, #15269, #13123 ) ;
#6905 = EDGE_CURVE ( 'NONE', #15200, #23082, #4084, .T. ) ;
#6906 = ADVANCED_FACE ( 'NONE', ( #20892 ), #14709, .F. ) ;
#6907 = DIRECTION ( 'NONE',  ( -1.000000000000000000, 0.000000000000000000, 0.000000000000000000 ) ) ;
#6908 = AXIS2_PLACEMENT_3D ( 'NONE', #331, #22179, #2803 ) ;
#6909 = CARTESIAN_POINT ( 'NONE',  ( -0.06894484415258525511, -0.05111597790624471116, -0.4724409448841456749 ) ) ;
#6910 = CARTESIAN_POINT ( 'NONE',  ( 0.07874015748031498729, -0.01181388133159171419, -0.4653549736499515421 ) ) ;
#6911 = CARTESIAN_POINT ( 'NONE',  ( 0.0006620872580302083164, 0.5229309616567520136, 0.1392975274215518533 ) ) ;
#6912 = CARTESIAN_POINT ( 'NONE',  ( 0.2268096725222374654, 0.4600326175560591202, 1.766732283464566899 ) ) ;
#6913 = ORIENTED_EDGE ( 'NONE', *, *, #13672, .T. ) ;
#6914 = DIRECTION ( 'NONE',  ( -1.000000000000000000, 0.000000000000000000, 0.000000000000000000 ) ) ;
#6915 = ORIENTED_EDGE ( 'NONE', *, *, #9352, .F. ) ;
#6916 = DIRECTION ( 'NONE',  ( 0.6427876096865391409, -0.7660444431189782355, 0.000000000000000000 ) ) ;
#6917 = DIRECTION ( 'NONE',  ( 1.000000000000000000, 0.000000000000000000, 0.000000000000000000 ) ) ;
#6918 = AXIS2_PLACEMENT_3D ( 'NONE', #178, #4517, #6917 ) ;
#6919 = ORIENTED_EDGE ( 'NONE', *, *, #11831, .T. ) ;
#6920 = CARTESIAN_POINT ( 'NONE',  ( 0.09842519685039370636, 0.5905905511811023745, -3.272637795275590733 ) ) ;
#6921 = VECTOR ( 'NONE', #8527, 39.37007874015748143 ) ;
#6922 = CARTESIAN_POINT ( 'NONE',  ( 0.1522836969735573143, 0.000000000000000000, 0.000000000000000000 ) ) ;
#6923 = FACE_OUTER_BOUND ( 'NONE', #21322, .T. ) ;
#6924 = EDGE_LOOP ( 'NONE', ( #9104, #18424 ) ) ;
#6925 = CARTESIAN_POINT ( 'NONE',  ( -0.5476281405333195407, -0.07214854559197286799, 0.9202755905511811330 ) ) ;
#6926 = AXIS2_PLACEMENT_3D ( 'NONE', #1384, #15935, #9718 ) ;
#6927 = DIMENSIONAL_EXPONENTS ( 1.000000000000000000, 0.000000000000000000, 0.000000000000000000, 0.000000000000000000, 0.000000000000000000, 0.000000000000000000, 0.000000000000000000 ) ;
#6928 = ORIENTED_EDGE ( 'NONE', *, *, #23042, .F. ) ;
#6929 = DIRECTION ( 'NONE',  ( 0.000000000000000000, 0.000000000000000000, 1.000000000000000000 ) ) ;
#6930 = EDGE_LOOP ( 'NONE', ( #8953, #14362 ) ) ;
#6931 = EDGE_CURVE ( 'NONE', #26797, #26980, #23457, .T. ) ;
#6932 = CIRCLE ( 'NONE', #7357, 0.5570866141732283561 ) ;
#6933 = SURFACE_SIDE_STYLE ('',( #26000 ) ) ;
#6934 = DIRECTION ( 'NONE',  ( 0.000000000000000000, 0.000000000000000000, 1.000000000000000000 ) ) ;
#6935 = CIRCLE ( 'NONE', #6029, 0.5007874015748031704 ) ;
#6936 = DIRECTION ( 'NONE',  ( 0.000000000000000000, 0.000000000000000000, -1.000000000000000000 ) ) ;
#6937 = CARTESIAN_POINT ( 'NONE',  ( 0.1120675189988344506, -0.4694218845611126678, -0.3846748511993472452 ) ) ;
#6938 = CARTESIAN_POINT ( 'NONE',  ( 0.03532354024591839031, -1.183070866141732402, 6.774128948039492984E-17 ) ) ;
#6939 = EDGE_CURVE ( 'NONE', #13078, #3782, #9931, .T. ) ;
#6940 = FACE_OUTER_BOUND ( 'NONE', #523, .T. ) ;
#6941 = CARTESIAN_POINT ( 'NONE',  ( 0.000000000000000000, 0.000000000000000000, 0.6299212598425196763 ) ) ;
#6942 = EDGE_CURVE ( 'NONE', #19742, #13676, #16508, .T. ) ;
#6943 = CLOSED_SHELL ( 'NONE', ( #464, #3069, #4060, #8477, #3244, #4726, #13143, #21782, #24844, #27055, #7859, #10937, #15660, #5154, #8461, #24780, #6552, #15723, #2674, #1726, #15050, #20764, #17607, #11427, #24289, #23830, #9727, #7669, #20923, #23178, #23527, #26593, #6399, #4713, #5220, #15053, #19864, #26550, #24917, #15310, #9513, #10160, #176, #26993, #7893, #8259, #23826, #11945, #6421, #15147, #4471, #20738, #1396, #15306 ) ) ;
#6944 = CARTESIAN_POINT ( 'NONE',  ( 0.000000000000000000, 0.000000000000000000, -0.05511811023622047168 ) ) ;
#6945 = CARTESIAN_POINT ( 'NONE',  ( -0.5708661417322835607, -0.03736310157554036115, 0.9399606299212598381 ) ) ;
#6946 = CARTESIAN_POINT ( 'NONE',  ( 0.06699590632655393063, -0.5118110236220473341, 1.766732283464566677 ) ) ;
#6947 = DIRECTION ( 'NONE',  ( 0.000000000000000000, 0.000000000000000000, 1.000000000000000000 ) ) ;
#6948 = LINE ( 'NONE', #208, #2434 ) ;
#6949 = EDGE_CURVE ( 'NONE', #11214, #26700, #14458, .T. ) ;
#6950 = VECTOR ( 'NONE', #5798, 39.37007874015748143 ) ;
#6951 = ORIENTED_EDGE ( 'NONE', *, *, #7556, .F. ) ;
#6952 = ORIENTED_EDGE ( 'NONE', *, *, #4024, .T. ) ;
#6953 = DIRECTION ( 'NONE',  ( 0.000000000000000000, -1.000000000000000000, 0.000000000000000000 ) ) ;
#6954 = CARTESIAN_POINT ( 'NONE',  ( 0.000000000000000000, 0.000000000000000000, 0.09685039370078740717 ) ) ;
#6955 = DIRECTION ( 'NONE',  ( 0.000000000000000000, 0.000000000000000000, 1.000000000000000000 ) ) ;
#6956 = CARTESIAN_POINT ( 'NONE',  ( 0.000000000000000000, 0.4232283464566928832, 0.1377952755905511861 ) ) ;
#6957 = ORIENTED_EDGE ( 'NONE', *, *, #5033, .F. ) ;
#6958 = AXIS2_PLACEMENT_3D ( 'NONE', #16284, #20938, #25166 ) ;
#6959 = FACE_OUTER_BOUND ( 'NONE', #1577, .T. ) ;
#6960 = ORIENTED_EDGE ( 'NONE', *, *, #25396, .T. ) ;
#6961 = FACE_BOUND ( 'NONE', #20194, .T. ) ;
#6962 = CARTESIAN_POINT ( 'NONE',  ( -0.6118597084614606496, 0.1076640027107484132, 0.09684793308443542803 ) ) ;
#6963 = CARTESIAN_POINT ( 'NONE',  ( 0.4895462770358314786, 0.6604130065488427181, -0.5726600247966424639 ) ) ;
#6964 = EDGE_CURVE ( 'NONE', #10366, #20882, #18007, .T. ) ;
#6965 = ( LENGTH_UNIT ( ) NAMED_UNIT ( * ) SI_UNIT ( $, .METRE. ) ) ;
#6966 = VECTOR ( 'NONE', #25462, 39.37007874015748143 ) ;
#6967 = B_SPLINE_CURVE_WITH_KNOTS ( 'NONE', 3,
 ( #20360, #9324, #26562, #16131, #7219, #15838 ),
 .UNSPECIFIED., .F., .F.,
 ( 4, 2, 4 ),
 ( 0.9031406754215589583, 0.9046454396443730506, 0.9061502038671860326 ),
 .UNSPECIFIED. ) ;
#6968 = AXIS2_PLACEMENT_3D ( 'NONE', #4319, #18763, #20758 ) ;
#6969 = CARTESIAN_POINT ( 'NONE',  ( 0.000000000000000000, 0.000000000000000000, 0.1322834645669291320 ) ) ;
#6970 = CARTESIAN_POINT ( 'NONE',  ( -0.5376957092749645728, -0.3112026930392425284, 0.09685039370078740717 ) ) ;
#6971 = CARTESIAN_POINT ( 'NONE',  ( -0.06699507805604322519, 0.5085118447796660446, -1.550196850393700920 ) ) ;
#6972 = EDGE_CURVE ( 'NONE', #25110, #22690, #13514, .T. ) ;
#6973 = CARTESIAN_POINT ( 'NONE',  ( 0.03001016326913580681, 0.4585215200179055817, -1.928289503579156516 ) ) ;
#6974 = ORIENTED_EDGE ( 'NONE', *, *, #3528, .F. ) ;
#6975 = CARTESIAN_POINT ( 'NONE',  ( 0.3030032861724964444, -0.3454440660767522098, -1.928289503579156516 ) ) ;
#6976 = CARTESIAN_POINT ( 'NONE',  ( -0.1775991818008739453, 0.5230301363771271417, 0.9202755905511811330 ) ) ;
#6977 = CARTESIAN_POINT ( 'NONE',  ( -0.5385210225480960844, 0.4284847435812472183, 0.1322834645669291320 ) ) ;
#6978 = AXIS2_PLACEMENT_3D ( 'NONE', #20907, #22894, #25283 ) ;
#6979 = CARTESIAN_POINT ( 'NONE',  ( 0.2305483297598421022, -0.4797636960996590760, 0.3401591244667909186 ) ) ;
#6980 = CARTESIAN_POINT ( 'NONE',  ( -0.6208708315385689236, -0.08043444190496674973, -0.2401670989486988372 ) ) ;
#6981 = CARTESIAN_POINT ( 'NONE',  ( 0.000000000000000000, 0.000000000000000000, 0.3425196850393700809 ) ) ;
#6982 = FACE_BOUND ( 'NONE', #1206, .T. ) ;
#6983 = CARTESIAN_POINT ( 'NONE',  ( -0.4067073728345788064, -0.2341441294389334793, 0.1992125984251968684 ) ) ;
#6984 = AXIS2_PLACEMENT_3D ( 'NONE', #26690, #22465, #18627 ) ;
#6985 = DIRECTION ( 'NONE',  ( 1.000000000000000000, 0.000000000000000000, 0.000000000000000000 ) ) ;
#6986 = CONICAL_SURFACE ( 'NONE', #4710, 0.1106489370078740930, 0.08726646250000029414 ) ;
#6987 = DIRECTION ( 'NONE',  ( 1.000000000000000000, 0.000000000000000000, 0.000000000000000000 ) ) ;
#6988 = ORIENTED_EDGE ( 'NONE', *, *, #9138, .F. ) ;
#6989 = CARTESIAN_POINT ( 'NONE',  ( 0.3996755081323252745, 0.4756294029998354156, 0.2574819594177527593 ) ) ;
#6990 = ORIENTED_EDGE ( 'NONE', *, *, #16984, .T. ) ;
#6991 = CARTESIAN_POINT ( 'NONE',  ( -0.7121770198535963825, 0.1804934768145626256, 0.06452349730229350877 ) ) ;
#6992 = ORIENTED_EDGE ( 'NONE', *, *, #21821, .T. ) ;
#6993 = EDGE_CURVE ( 'NONE', #24685, #19453, #6782, .T. ) ;
#6994 = PLANE ( 'NONE',  #16526 ) ;
#6995 = CYLINDRICAL_SURFACE ( 'NONE', #508, 0.1181102362204720091 ) ;
#6996 = EDGE_CURVE ( 'NONE', #14064, #16332, #13083, .T. ) ;
#6997 = CIRCLE ( 'NONE', #24127, 0.6299212598425196763 ) ;
#6998 = DIRECTION ( 'NONE',  ( 0.000000000000000000, 0.000000000000000000, -1.000000000000000000 ) ) ;
#6999 = CARTESIAN_POINT ( 'NONE',  ( 0.3644697409450263215, 0.09762295995069791843, -3.100567304031765836 ) ) ;
#7000 = CARTESIAN_POINT ( 'NONE',  ( -0.09139240964747707974, -0.07874015748031502893, 0.02109836160874977232 ) ) ;
#7001 = DIRECTION ( 'NONE',  ( 1.000000000000000000, 0.000000000000000000, 0.000000000000000000 ) ) ;
#7002 = FACE_OUTER_BOUND ( 'NONE', #15517, .T. ) ;
#7003 = ORIENTED_EDGE ( 'NONE', *, *, #4708, .F. ) ;
#7004 = CARTESIAN_POINT ( 'NONE',  ( -0.4921259842519685179, 3.013402556957069934E-17, -1.569881889763779625 ) ) ;
#7005 = AXIS2_PLACEMENT_3D ( 'NONE', #24131, #23997, #26117 ) ;
#7006 = AXIS2_PLACEMENT_3D ( 'NONE', #19227, #2401, #25449 ) ;
#7007 = CARTESIAN_POINT ( 'NONE',  ( -0.2297883689023225706, -0.3979194638820617858, -1.928289503579150077 ) ) ;
#7008 = EDGE_LOOP ( 'NONE', ( #11460, #1209, #6288, #16790 ) ) ;
#7009 = CARTESIAN_POINT ( 'NONE',  ( 0.4021324607176451904, 0.3215300179777050293, 0.3251195115651615564 ) ) ;
#7010 = DIRECTION ( 'NONE',  ( 0.000000000000000000, 0.000000000000000000, 1.000000000000000000 ) ) ;
#7011 = DIRECTION ( 'NONE',  ( 0.000000000000000000, 0.000000000000000000, 1.000000000000000000 ) ) ;
#7012 = CARTESIAN_POINT ( 'NONE',  ( -0.3855916753051397139, 0.3382184156732160329, 1.747047244094488194 ) ) ;
#7013 = AXIS2_PLACEMENT_3D ( 'NONE', #26658, #20166, #26383 ) ;
#7014 = DIRECTION ( 'NONE',  ( 0.000000000000000000, 0.000000000000000000, -1.000000000000000000 ) ) ;
#7015 = ORIENTED_EDGE ( 'NONE', *, *, #18973, .T. ) ;
#7016 = B_SPLINE_CURVE_WITH_KNOTS ( 'NONE', 3,
 ( #13026, #10910, #13305, #19532, #21930, #4279 ),
 .UNSPECIFIED., .F., .F.,
 ( 4, 2, 4 ),
 ( 0.2376120521391529850, 0.2390783382518550104, 0.2405446243645580073 ),
 .UNSPECIFIED. ) ;
#7017 = CARTESIAN_POINT ( 'NONE',  ( 0.1867299569291683836, 0.3233561589689052940, -3.115157480314960647 ) ) ;
#7018 = VERTEX_POINT ( 'NONE', #14415 ) ;
#7019 = CARTESIAN_POINT ( 'NONE',  ( -0.01968503937007897581, 0.000000000000000000, 0.000000000000000000 ) ) ;
#7020 = CARTESIAN_POINT ( 'NONE',  ( 0.4837521785364486404, -0.1097523286759638783, 0.1734435147541967814 ) ) ;
#7021 = CARTESIAN_POINT ( 'NONE',  ( 0.08676778863011423704, 0.3239425792934499948, 1.953740157480315043 ) ) ;
#7022 = ORIENTED_EDGE ( 'NONE', *, *, #10581, .F. ) ;
#7023 = CIRCLE ( 'NONE', #8809, 0.3937007874015748254 ) ;
#7024 = CARTESIAN_POINT ( 'NONE',  ( -0.2066929133858267931, 0.000000000000000000, 0.000000000000000000 ) ) ;
#7025 = VECTOR ( 'NONE', #13303, 39.37007874015748854 ) ;
#7026 = ORIENTED_EDGE ( 'NONE', *, *, #16884, .T. ) ;
#7027 = DIRECTION ( 'NONE',  ( 0.000000000000000000, 0.000000000000000000, 1.000000000000000000 ) ) ;
#7028 = EDGE_CURVE ( 'NONE', #724, #18101, #4952, .T. ) ;
#7029 = CIRCLE ( 'NONE', #21936, 0.5322834645669292097 ) ;
#7030 = CARTESIAN_POINT ( 'NONE',  ( 0.3843128886798082844, 0.1418101685954901714, -0.2362204724409449064 ) ) ;
#7031 = FACE_OUTER_BOUND ( 'NONE', #4030, .T. ) ;
#7032 = CARTESIAN_POINT ( 'NONE',  ( 0.000000000000000000, 0.000000000000000000, 0.1992125984251968684 ) ) ;
#7033 = ORIENTED_EDGE ( 'NONE', *, *, #746, .T. ) ;
#7034 = CIRCLE ( 'NONE', #26415, 0.01377952755905510404 ) ;
#7035 = DIRECTION ( 'NONE',  ( -0.5518027697606309179, 0.000000000000000000, 0.8339746418713797071 ) ) ;
#7036 = CARTESIAN_POINT ( 'NONE',  ( -0.3184841198566451537, -0.1570220809524492667, 1.953740157480315043 ) ) ;
#7037 = CARTESIAN_POINT ( 'NONE',  ( -0.2126900928101059240, -0.5837180524351401889, 0.09684793308443542803 ) ) ;
#7038 = CARTESIAN_POINT ( 'NONE',  ( 0.1501355178992943573, 0.2127853528708066044, -0.4344888834448818460 ) ) ;
#7039 = CARTESIAN_POINT ( 'NONE',  ( 0.000000000000000000, -0.09092130223458683158, -0.3779527559055118058 ) ) ;
#7040 = AXIS2_PLACEMENT_3D ( 'NONE', #19213, #4247, #25718 ) ;
#7041 = DIRECTION ( 'NONE',  ( 0.000000000000000000, 1.000000000000000000, 0.000000000000000000 ) ) ;
#7042 = CARTESIAN_POINT ( 'NONE',  ( 0.06889763779527550980, 0.000000000000000000, -0.2834645669291338543 ) ) ;
#7043 = ADVANCED_FACE ( 'NONE', ( #18761 ), #24810, .F. ) ;
#7044 = AXIS2_PLACEMENT_3D ( 'NONE', #7244, #5418, #15863 ) ;
#7045 = ORIENTED_EDGE ( 'NONE', *, *, #18252, .F. ) ;
#7046 = CARTESIAN_POINT ( 'NONE',  ( -0.2362204724409449064, -1.131889763779527547, 1.386165176200252194E-16 ) ) ;
#7047 = VERTEX_POINT ( 'NONE', #23024 ) ;
#7048 = DIRECTION ( 'NONE',  ( 0.000000000000000000, 0.7071067811865474617, 0.7071067811865474617 ) ) ;
#7049 = CARTESIAN_POINT ( 'NONE',  ( -0.4783464566929133688, -0.4724409448818898127, 0.6411263657805729155 ) ) ;
#7050 = ORIENTED_EDGE ( 'NONE', *, *, #1186, .F. ) ;
#7051 = CARTESIAN_POINT ( 'NONE',  ( -0.4932821129636645874, 0.08637579872942342807, 0.2574803149606298969 ) ) ;
#7052 = ORIENTED_EDGE ( 'NONE', *, *, #15524, .F. ) ;
#7053 = B_SPLINE_CURVE_WITH_KNOTS ( 'NONE', 3,
 ( #5494, #16497, #3490, #18604, #10136, #27245, #10274, #14262 ),
 .UNSPECIFIED., .F., .F.,
 ( 4, 2, 2, 4 ),
 ( 0.000000000000000000, 0.2500000000000000000, 0.5000000000000000000, 1.000000000000000000 ),
 .UNSPECIFIED. ) ;
#7054 = CARTESIAN_POINT ( 'NONE',  ( -0.03532354024591775193, -1.183070866141732402, 6.774128948039492984E-17 ) ) ;
#7055 = CARTESIAN_POINT ( 'NONE',  ( -0.3411065095061437957, 0.06065137456822555090, 0.1377952755905512139 ) ) ;
#7056 = EDGE_CURVE ( 'NONE', #14958, #1047, #22672, .T. ) ;
#7057 = VERTEX_POINT ( 'NONE', #27543 ) ;
#7058 = CARTESIAN_POINT ( 'NONE',  ( -0.3642352168757148623, 0.4152525734086685016, 0.9399606299212598381 ) ) ;
#7059 = EDGE_LOOP ( 'NONE', ( #3335, #3816, #12558, #872, #3485 ) ) ;
#7060 = PLANE ( 'NONE',  #20298 ) ;
#7061 = ORIENTED_EDGE ( 'NONE', *, *, #8900, .T. ) ;
#7062 = DIRECTION ( 'NONE',  ( 0.000000000000000000, -1.000000000000000000, 0.000000000000000000 ) ) ;
#7063 = PRODUCT_DEFINITION_FORMATION_WITH_SPECIFIED_SOURCE ( 'ANY', '', #19280, .NOT_KNOWN. ) ;
#7064 = CIRCLE ( 'NONE', #12020, 0.01377952755905511792 ) ;
#7065 = DIRECTION ( 'NONE',  ( 1.000000000000000000, 0.000000000000000000, 0.000000000000000000 ) ) ;
#7066 = DIRECTION ( 'NONE',  ( 0.000000000000000000, 0.000000000000000000, -1.000000000000000000 ) ) ;
#7067 = DIRECTION ( 'NONE',  ( -0.000000000000000000, -1.000000000000000000, -0.000000000000000000 ) ) ;
#7068 = CARTESIAN_POINT ( 'NONE',  ( -0.4015002836674314013, -0.2311469024290320751, 0.2048502514845859379 ) ) ;
#7069 = CIRCLE ( 'NONE', #26928, 0.6889763779527560139 ) ;
#7070 = CARTESIAN_POINT ( 'NONE',  ( -6.132876883919029269E-17, -0.5007874015748031704, -3.278217716535432842E-17 ) ) ;
#7071 = DIRECTION ( 'NONE',  ( 1.000000000000000000, 0.000000000000000000, 0.000000000000000000 ) ) ;
#7072 = CARTESIAN_POINT ( 'NONE',  ( 0.3007905576423755556, -0.1482986320106471911, 1.953740157480315043 ) ) ;
#7073 = ORIENTED_EDGE ( 'NONE', *, *, #18790, .F. ) ;
#7074 = CARTESIAN_POINT ( 'NONE',  ( -0.5905511811023621549, -1.131889763779527547, 1.386165176200252194E-16 ) ) ;
#7075 = CARTESIAN_POINT ( 'NONE',  ( 0.4980314960629921295, 6.183502046875907854E-17, -6.010066929133858501E-17 ) ) ;
#7076 = EDGE_CURVE ( 'NONE', #21302, #21339, #20095, .T. ) ;
#7077 = CARTESIAN_POINT ( 'NONE',  ( 0.4954156765914815574, -0.2860899518037339773, 0.9399606299212598381 ) ) ;
#7078 = CARTESIAN_POINT ( 'NONE',  ( 0.3145317858139327627, -0.4092783051644229841, 1.766732283464566899 ) ) ;
#7079 = CARTESIAN_POINT ( 'NONE',  ( 0.5869493968219645641, 0.000000000000000000, 0.000000000000000000 ) ) ;
#7080 = CARTESIAN_POINT ( 'NONE',  ( 0.000000000000000000, 0.000000000000000000, 0.2637795275590551491 ) ) ;
#7081 = CARTESIAN_POINT ( 'NONE',  ( -0.4681308612729632723, -0.1074986424507606286, 0.2194422276514244319 ) ) ;
#7082 = EDGE_CURVE ( 'NONE', #4795, #4592, #6895, .T. ) ;
#7083 = EDGE_LOOP ( 'NONE', ( #25016, #2761, #459, #20214 ) ) ;
#7084 = EDGE_CURVE ( 'NONE', #4895, #23052, #4226, .T. ) ;
#7085 = ADVANCED_FACE ( 'NONE', ( #13245, #23864 ), #4360, .T. ) ;
#7086 = ORIENTED_EDGE ( 'NONE', *, *, #2115, .F. ) ;
#7087 = AXIS2_PLACEMENT_3D ( 'NONE', #21756, #15546, #313 ) ;
#7088 = VECTOR ( 'NONE', #12358, 39.37007874015748143 ) ;
#7089 = LINE ( 'NONE', #4956, #11983 ) ;
#7090 = ADVANCED_FACE ( 'NONE', ( #24122 ), #23591, .T. ) ;
#7091 = CARTESIAN_POINT ( 'NONE',  ( -0.4599954779395757920, 0.2268956277328612881, -1.550196850393700920 ) ) ;
#7092 = FACE_OUTER_BOUND ( 'NONE', #437, .T. ) ;
#7093 = ORIENTED_EDGE ( 'NONE', *, *, #3867, .F. ) ;
#7094 = LENGTH_MEASURE_WITH_UNIT ( LENGTH_MEASURE( 0.02539999999999999897 ), #13574 ) ;
#7095 = CARTESIAN_POINT ( 'NONE',  ( -0.3174445073348015067, -0.1826860508804799832, 0.08455817587939960800 ) ) ;
#7096 = CARTESIAN_POINT ( 'NONE',  ( 0.7874015748031325534, 0.2480907742005069583, -0.2781032352068246172 ) ) ;
#7097 = CARTESIAN_POINT ( 'NONE',  ( 0.2952755905264887182, 0.000000000000000000, -3.110236220451535694 ) ) ;
#7098 = DIRECTION ( 'NONE',  ( 1.000000000000000000, 0.000000000000000000, 0.000000000000000000 ) ) ;
#7099 = VERTEX_POINT ( 'NONE', #4757 ) ;
#7100 = CIRCLE ( 'NONE', #14817, 0.6193720790381457286 ) ;
#7101 = CYLINDRICAL_SURFACE ( 'NONE', #15711, 0.4921259842519685179 ) ;
#7102 = DIRECTION ( 'NONE',  ( -1.000000000000000000, 0.000000000000000000, 0.000000000000000000 ) ) ;
#7103 = CARTESIAN_POINT ( 'NONE',  ( -0.3979194638820449104, -0.2297883689023288989, -1.928289503579160513 ) ) ;
#7104 = B_SPLINE_CURVE_WITH_KNOTS ( 'NONE', 3,
 ( #15325, #6411, #15038, #4289, #26034, #23654 ),
 .UNSPECIFIED., .F., .F.,
 ( 4, 2, 4 ),
 ( 0.9359046326925629655, 0.9375808709372039917, 0.9392571091818440188 ),
 .UNSPECIFIED. ) ;
#7105 = DIRECTION ( 'NONE',  ( 0.000000000000000000, 1.000000000000000000, 0.000000000000000000 ) ) ;
#7106 = CARTESIAN_POINT ( 'NONE',  ( -9.506830708661417994E-16, -0.8267716535433071723, 0.000000000000000000 ) ) ;
#7107 = CARTESIAN_POINT ( 'NONE',  ( -0.4561454261039838420, 0.08101060747556922126, 0.2048502514525085139 ) ) ;
#7108 = EDGE_CURVE ( 'NONE', #12714, #13350, #12641, .T. ) ;
#7109 = CARTESIAN_POINT ( 'NONE',  ( -0.6544535166833030937, -0.004815824195081693654, -0.07874015109845866611 ) ) ;
#7110 = CARTESIAN_POINT ( 'NONE',  ( 0.1718374205099799101, -0.4703827404237102550, 0.2574803149606298969 ) ) ;
#7111 = ADVANCED_FACE ( 'NONE', ( #21870 ), #19189, .F. ) ;
#7112 = CARTESIAN_POINT ( 'NONE',  ( 0.03532354024591712049, -0.8267716535433071723, 0.000000000000000000 ) ) ;
#7113 = CARTESIAN_POINT ( 'NONE',  ( -0.0006832381873097717172, 0.6614169699448725348, 0.1926811207749853927 ) ) ;
#7114 = PRODUCT_DEFINITION_FORMATION_WITH_SPECIFIED_SOURCE ( 'ANY', '', #163, .NOT_KNOWN. ) ;
#7115 = DIRECTION ( 'NONE',  ( 0.3420201433256690460, -0.9396926207859084279, 0.000000000000000000 ) ) ;
#7116 = CIRCLE ( 'NONE', #391, 0.3464566929133857665 ) ;
#7117 = CARTESIAN_POINT ( 'NONE',  ( 0.000000000000000000, 0.000000000000000000, 0.2362204724409449064 ) ) ;
#7118 = VERTEX_POINT ( 'NONE', #17622 ) ;
#7119 = CARTESIAN_POINT ( 'NONE',  ( 0.2341075107471200512, 0.2669897767696595703, 1.953740157480315043 ) ) ;
#7120 = EDGE_LOOP ( 'NONE', ( #740, #15771, #18224, #16093 ) ) ;
#7121 = CARTESIAN_POINT ( 'NONE',  ( 0.4382752542995623779, 0.1173917140416305405, -1.934055118110236338 ) ) ;
#7122 = DIRECTION ( 'NONE',  ( 1.000000000000000000, 7.017815000000030939E-18, 0.000000000000000000 ) ) ;
#7123 = CARTESIAN_POINT ( 'NONE',  ( -0.1918813796216842782, -0.5271897577243779276, 0.1771653543307086520 ) ) ;
#7124 = DIRECTION ( 'NONE',  ( -0.5000000000000001110, 0.8660254037844384856, 0.000000000000000000 ) ) ;
#7125 = CARTESIAN_POINT ( 'NONE',  ( 0.0005696707463077370576, 0.4606295689977898400, 0.1771653543307089018 ) ) ;
#7126 = B_SPLINE_CURVE_WITH_KNOTS ( 'NONE', 3,
 ( #18186, #26826, #18618, #7476, #5508, #16104, #5360, #9733, #27123, #7769 ),
 .UNSPECIFIED., .F., .F.,
 ( 4, 2, 2, 2, 4 ),
 ( 0.000000000000000000, 0.2500000000000000000, 0.5000000000000000000, 0.7500000000000000000, 1.000000000000000000 ),
 .UNSPECIFIED. ) ;
#7127 = DIRECTION ( 'NONE',  ( 0.000000000000000000, 0.000000000000000000, -1.000000000000000000 ) ) ;
#7128 = CARTESIAN_POINT ( 'NONE',  ( 0.000000000000000000, 0.07874015748031491790, -1.811023622047243542 ) ) ;
#7129 = CARTESIAN_POINT ( 'NONE',  ( -0.3349073414798397486, -0.1651192144506304638, -3.115157480314960647 ) ) ;
#7130 = DIRECTION ( 'NONE',  ( 0.000000000000000000, 1.000000000000000000, 0.000000000000000000 ) ) ;
#7131 = CARTESIAN_POINT ( 'NONE',  ( 0.1490609433537086470, 0.2477131595981420797, 0.4096305452796897839 ) ) ;
#7132 = AXIS2_PLACEMENT_3D ( 'NONE', #13136, #17519, #6794 ) ;
#7133 = ORIENTED_EDGE ( 'NONE', *, *, #18122, .T. ) ;
#7134 = FACE_OUTER_BOUND ( 'NONE', #27240, .T. ) ;
#7135 = AXIS2_PLACEMENT_3D ( 'NONE', #17256, #25596, #19660 ) ;
#7136 = VECTOR ( 'NONE', #4690, 39.37007874015748854 ) ;
#7137 = APPLICATION_PROTOCOL_DEFINITION ( 'draft international standard', 'automotive_design', 1998, #22258 ) ;
#7138 = ADVANCED_FACE ( 'NONE', ( #2362 ), #12508, .F. ) ;
#7139 = ORIENTED_EDGE ( 'NONE', *, *, #15537, .T. ) ;
#7140 = AXIS2_PLACEMENT_3D ( 'NONE', #3235, #26845, #5384 ) ;
#7141 = ORIENTED_EDGE ( 'NONE', *, *, #1718, .F. ) ;
#7142 = CARTESIAN_POINT ( 'NONE',  ( -0.4157391792961063204, 0.3323952789219086768, 0.1322834645669291320 ) ) ;
#7143 = CARTESIAN_POINT ( 'NONE',  ( -0.6205616028481958368, -0.4724399524669597450, 0.9954595399567032210 ) ) ;
#7144 = CARTESIAN_POINT ( 'NONE',  ( -0.2564944395515793563, -0.4441657790107725323, 1.747047244094488194 ) ) ;
#7145 = EDGE_CURVE ( 'NONE', #18891, #19141, #26171, .T. ) ;
#7146 = DIRECTION ( 'NONE',  ( -0.9790454724845842893, 0.1018208755700880375, 0.1763589297585410332 ) ) ;
#7147 = ORIENTED_EDGE ( 'NONE', *, *, #1340, .F. ) ;
#7148 = CARTESIAN_POINT ( 'NONE',  ( -0.1867299569291685502, -0.3233561589689051829, -3.115157480314960647 ) ) ;
#7149 = DIRECTION ( 'NONE',  ( 0.000000000000000000, 0.000000000000000000, 1.000000000000000000 ) ) ;
#7150 = CARTESIAN_POINT ( 'NONE',  ( -0.07217847769028858107, -4.927204724409449161E-18, 0.000000000000000000 ) ) ;
#7151 = CARTESIAN_POINT ( 'NONE',  ( 0.000000000000000000, 0.000000000000000000, 0.3401574803149606252 ) ) ;
#7152 = AXIS2_PLACEMENT_3D ( 'NONE', #15250, #21737, #17080 ) ;
#7153 = CARTESIAN_POINT ( 'NONE',  ( 0.2211428102655795813, -0.2521176338356631019, 1.953740157480315043 ) ) ;
#7154 = EDGE_LOOP ( 'NONE', ( #5120, #7356, #26951, #7279, #1477 ) ) ;
#7155 = CIRCLE ( 'NONE', #20236, 0.3872945158171015589 ) ;
#7156 = CARTESIAN_POINT ( 'NONE',  ( 0.000000000000000000, 0.000000000000000000, 0.6228346456772185791 ) ) ;
#7157 = CONICAL_SURFACE ( 'NONE', #7629, 2.066929133858267598, 0.7853981624999996081 ) ;
#7158 = ORIENTED_EDGE ( 'NONE', *, *, #18869, .T. ) ;
#7159 = ORIENTED_EDGE ( 'NONE', *, *, #17574, .T. ) ;
#7160 = ORIENTED_EDGE ( 'NONE', *, *, #17780, .F. ) ;
#7161 = CARTESIAN_POINT ( 'NONE',  ( -0.01027864967283271050, 0.1968503937007874127, -3.626971312343105325 ) ) ;
#7162 = EDGE_CURVE ( 'NONE', #26868, #20801, #19748, .T. ) ;
#7163 = DIRECTION ( 'NONE',  ( 0.000000000000000000, 0.000000000000000000, 1.000000000000000000 ) ) ;
#7164 = CARTESIAN_POINT ( 'NONE',  ( -0.01027864967366022390, 0.1968503937007874127, -3.193900446201109578 ) ) ;
#7165 = VECTOR ( 'NONE', #18715, 39.37007874015748143 ) ;
#7166 = PLANE ( 'NONE',  #26346 ) ;
#7167 = CARTESIAN_POINT ( 'NONE',  ( -0.02576258704323624443, 0.2165354330708661457, -3.176774342847608512 ) ) ;
#7168 = DIRECTION ( 'NONE',  ( 1.000000000000000000, 0.000000000000000000, 0.000000000000000000 ) ) ;
#7169 = CARTESIAN_POINT ( 'NONE',  ( 0.2161381151963039093, -0.2817310484609168442, 1.953740157480315043 ) ) ;
#7170 = VECTOR ( 'NONE', #26388, 39.37007874015748854 ) ;
#7171 = CARTESIAN_POINT ( 'NONE',  ( -0.2305483297598421022, -0.4797636960996590760, 0.1322818204150988386 ) ) ;
#7172 = VECTOR ( 'NONE', #25980, 39.37007874015748143 ) ;
#7173 = FACE_OUTER_BOUND ( 'NONE', #25395, .T. ) ;
#7174 = DIRECTION ( 'NONE',  ( 0.000000000000000000, 0.000000000000000000, 1.000000000000000000 ) ) ;
#7175 = CARTESIAN_POINT ( 'NONE',  ( 0.06699507805368110080, -0.5085118447801203478, 1.747047244094488194 ) ) ;
#7176 = B_SPLINE_CURVE_WITH_KNOTS ( 'NONE', 3,
 ( #9882, #24853, #15692, #2804, #26542, #12007 ),
 .UNSPECIFIED., .F., .F.,
 ( 4, 2, 4 ),
 ( 0.2376120521391529850, 0.2390783382518560096, 0.2405446243645580073 ),
 .UNSPECIFIED. ) ;
#7177 = EDGE_CURVE ( 'NONE', #7047, #16467, #13998, .T. ) ;
#7178 = EDGE_LOOP ( 'NONE', ( #23080, #658, #20468, #4678 ) ) ;
#7179 = EDGE_CURVE ( 'NONE', #12355, #14847, #8132, .T. ) ;
#7180 = CARTESIAN_POINT ( 'NONE',  ( 0.4143458349590511403, -0.2398979215377306518, 0.1920935997039191212 ) ) ;
#7181 = EDGE_LOOP ( 'NONE', ( #18090, #23493 ) ) ;
#7182 = CARTESIAN_POINT ( 'NONE',  ( 2.664928230027803213, -0.4724409448818898127, 0.8182917201112815953 ) ) ;
#7183 = CARTESIAN_POINT ( 'NONE',  ( 0.09193072188197352890, -0.3429848536917953217, 1.953740157480315043 ) ) ;
#7184 = VERTEX_POINT ( 'NONE', #21594 ) ;
#7185 = ORIENTED_EDGE ( 'NONE', *, *, #5197, .T. ) ;
#7186 = CARTESIAN_POINT ( 'NONE',  ( -0.3912931228432220410, 0.3001918266902144361, -1.569881889763779625 ) ) ;
#7187 = CARTESIAN_POINT ( 'NONE',  ( 0.6993003464534486291, -0.1604063846362702717, 0.1601585119470639862 ) ) ;
#7188 = B_SPLINE_CURVE_WITH_KNOTS ( 'NONE', 3,
 ( #9928, #3708, #21090, #20949, #27743, #7823, #25612, #16431, #21379, #25048 ),
 .UNSPECIFIED., .F., .F.,
 ( 4, 2, 2, 2, 4 ),
 ( 0.000000000000000000, 0.2500000000000000000, 0.5000000000000000000, 0.7500000000000000000, 1.000000000000000000 ),
 .UNSPECIFIED. ) ;
#7189 = VERTEX_POINT ( 'NONE', #2230 ) ;
#7190 = CARTESIAN_POINT ( 'NONE',  ( -0.5417097841048968965, 0.1839420097223028183, 0.9399606299212598381 ) ) ;
#7191 = VERTEX_POINT ( 'NONE', #10853 ) ;
#7192 = DIRECTION ( 'NONE',  ( 0.000000000000000000, 0.000000000000000000, 1.000000000000000000 ) ) ;
#7193 = FACE_OUTER_BOUND ( 'NONE', #20077, .T. ) ;
#7194 = ITEM_DEFINED_TRANSFORMATION ( 'NONE', 'NONE', #11603,  #11588 ) ;
#7195 = LINE ( 'NONE', #9435, #9456 ) ;
#7196 = DIRECTION ( 'NONE',  ( 1.000000000000000000, 0.000000000000000000, 0.000000000000000000 ) ) ;
#7197 = FACE_OUTER_BOUND ( 'NONE', #21819, .T. ) ;
#7199 = CIRCLE ( 'NONE', #9438, 0.7500000000000001110 ) ;
#7198 = CARTESIAN_POINT ( 'NONE',  ( 0.000000000000000000, 0.000000000000000000, 0.4488188976377953110 ) ) ;
#7200 = EDGE_CURVE ( 'NONE', #478, #3160, #17594, .T. ) ;
#7201 = DIRECTION ( 'NONE',  ( -3.508908000000002129E-18, 0.5000000000000003331, 0.8660254037844384856 ) ) ;
#7202 = CARTESIAN_POINT ( 'NONE',  ( 0.009795313329541911057, 0.08526597544697904485, -0.4724409448818898127 ) ) ;
#7203 = DIRECTION ( 'NONE',  ( 0.000000000000000000, -0.7626852297620279053, -0.6467698511084468693 ) ) ;
#7204 = CARTESIAN_POINT ( 'NONE',  ( 0.6711032387266713251, -0.1523958994812761869, 0.3401574803149606252 ) ) ;
#7205 = CARTESIAN_POINT ( 'NONE',  ( 0.000000000000000000, 0.6102362204724409711, -1.156053543307086666E-17 ) ) ;
#7206 = CARTESIAN_POINT ( 'NONE',  ( -0.3145317858139328737, -0.4092783051644231507, 1.766732283464567121 ) ) ;
#7207 = DIRECTION ( 'NONE',  ( 1.000000000000000000, 0.000000000000000000, 0.000000000000000000 ) ) ;
#7208 = FACE_OUTER_BOUND ( 'NONE', #8008, .T. ) ;
#7209 = CIRCLE ( 'NONE', #9453, 0.4685039370078740717 ) ;
#7210 = EDGE_LOOP ( 'NONE', ( #10542, #1722, #26476 ) ) ;
#7211 = EDGE_LOOP ( 'NONE', ( #85, #24786 ) ) ;
#7212 = CIRCLE ( 'NONE', #112, 0.3070866141732283561 ) ;
#7213 = CYLINDRICAL_SURFACE ( 'NONE', #302, 0.09679133858267717494 ) ;
#7214 = CARTESIAN_POINT ( 'NONE',  ( 0.5981657849660177995, 0.000000000000000000, 0.000000000000000000 ) ) ;
#7215 = CARTESIAN_POINT ( 'NONE',  ( -0.07874015747999545123, 0.1968503937007873850, -3.558537267005807525 ) ) ;
#7216 = ORIENTED_EDGE ( 'NONE', *, *, #19235, .F. ) ;
#7217 = CARTESIAN_POINT ( 'NONE',  ( 0.000000000000000000, 0.000000000000000000, 0.01181102362204724393 ) ) ;
#7218 = ORIENTED_EDGE ( 'NONE', *, *, #24541, .F. ) ;
#7219 = CARTESIAN_POINT ( 'NONE',  ( 0.4338922498494567348, -0.2500511477696476526, 0.2574819596263889787 ) ) ;
#7220 = DIMENSIONAL_EXPONENTS ( 1.000000000000000000, 0.000000000000000000, 0.000000000000000000, 0.000000000000000000, 0.000000000000000000, 0.000000000000000000, 0.000000000000000000 ) ;
#7221 = CARTESIAN_POINT ( 'NONE',  ( 0.7871730179869745880, 0.2557924603599555091, -0.2773276354974251734 ) ) ;
#7222 = ADVANCED_FACE ( 'NONE', ( #18294 ), #23038, .F. ) ;
#7223 = AXIS2_PLACEMENT_3D ( 'NONE', #22839, #6033, #10243 ) ;
#7224 = CARTESIAN_POINT ( 'NONE',  ( 0.04928528614549729930, 0.3765118517642103702, -3.100567304031763172 ) ) ;
#7225 = FACE_OUTER_BOUND ( 'NONE', #28, .T. ) ;
#7226 = ORIENTED_EDGE ( 'NONE', *, *, #20478, .F. ) ;
#7227 = CARTESIAN_POINT ( 'NONE',  ( 0.1078280746904042159, 0.3175540113612283499, 1.973425196850393970 ) ) ;
#7228 = CARTESIAN_POINT ( 'NONE',  ( 0.4423390553432353656, -0.2180862235769564228, -1.550196850393700920 ) ) ;
#7229 = EDGE_CURVE ( 'NONE', #16925, #26228, #10851, .T. ) ;
#7230 = CARTESIAN_POINT ( 'NONE',  ( 0.4585215200179055817, 0.03001016326913595253, -1.928289503579156516 ) ) ;
#7231 = AXIS2_PLACEMENT_3D ( 'NONE', #24459, #5112, #13736 ) ;
#7232 = CARTESIAN_POINT ( 'NONE',  ( -0.5230301363771709955, 0.1775991818008312573, 0.9399606299212598381 ) ) ;
#7233 = CARTESIAN_POINT ( 'NONE',  ( -0.07874015748031511219, 0.1968503937007874127, -3.548228346456693050 ) ) ;
#7234 = ADVANCED_FACE ( 'NONE', ( #13652 ), #26641, .F. ) ;
#7235 = CARTESIAN_POINT ( 'NONE',  ( 1.687505431895960050E-16, 0.07874015748031508444, 1.377952755905512472 ) ) ;
#7236 = CARTESIAN_POINT ( 'NONE',  ( 0.3200513472077004540, 0.3804946224888235418, 0.1140743250920687596 ) ) ;
#7237 = CARTESIAN_POINT ( 'NONE',  ( -0.3912931228432220410, 0.3001918266902144361, -1.569881889763779625 ) ) ;
#7238 = CARTESIAN_POINT ( 'NONE',  ( -0.4055118110236220486, -0.4724409448818898127, -0.6411263657805729155 ) ) ;
#7239 = CARTESIAN_POINT ( 'NONE',  ( 0.3905379133858267737, -0.2805118110236220486, -0.4858607088160724063 ) ) ;
#7240 = DIRECTION ( 'NONE',  ( 0.000000000000000000, 0.000000000000000000, -1.000000000000000000 ) ) ;
#7241 = DIRECTION ( 'NONE',  ( 0.000000000000000000, 0.000000000000000000, 1.000000000000000000 ) ) ;
#7242 = DIRECTION ( 'NONE',  ( 0.000000000000000000, 1.000000000000000000, 0.000000000000000000 ) ) ;
#7243 = ( NAMED_UNIT ( * ) PLANE_ANGLE_UNIT ( ) SI_UNIT ( $, .RADIAN. ) ) ;
#7244 = CARTESIAN_POINT ( 'NONE',  ( 0.5525004126151165096, 0.09742072959660433296, 0.1771653543307086520 ) ) ;
#7245 = CARTESIAN_POINT ( 'NONE',  ( -1.012503259137575512E-16, -0.8267716535433071723, 0.2362204724409449064 ) ) ;
#7246 = EDGE_LOOP ( 'NONE', ( #18457, #11037, #5960, #13093, #9921 ) ) ;
#7247 = CARTESIAN_POINT ( 'NONE',  ( 0.3075341118175934363, 0.1775236553382197324, 1.953740157480314821 ) ) ;
#7248 = ADVANCED_FACE ( 'NONE', ( #4898 ), #23595, .T. ) ;
#7249 = ORIENTED_EDGE ( 'NONE', *, *, #17017, .F. ) ;
#7250 = CARTESIAN_POINT ( 'NONE',  ( 0.05926487674659523808, -0.4498374011143459472, -1.934055118110236338 ) ) ;
#7251 = DIRECTION ( 'NONE',  ( -1.224646799147353207E-16, 1.000000000000000000, 0.000000000000000000 ) ) ;
#7252 = ORIENTED_EDGE ( 'NONE', *, *, #14176, .F. ) ;
#7253 = CARTESIAN_POINT ( 'NONE',  ( 0.5579526598176609564, -0.3213561723288210215, 0.1183902030407611161 ) ) ;
#7254 = CARTESIAN_POINT ( 'NONE',  ( 0.1490609433537086470, -0.2308938785792120918, 0.4193411617035458505 ) ) ;
#7255 = CARTESIAN_POINT ( 'NONE',  ( 0.3714952424334504455, 0.06515381386493819538, 0.07637630750536809898 ) ) ;
#7256 = DIRECTION ( 'NONE',  ( 1.000000000000000000, 0.000000000000000000, 0.000000000000000000 ) ) ;
#7257 = FACE_OUTER_BOUND ( 'NONE', #27624, .T. ) ;
#7258 = CYLINDRICAL_SURFACE ( 'NONE', #20200, 0.2952755905511805778 ) ;
#7259 = ADVANCED_FACE ( 'NONE', ( #13509 ), #7434, .F. ) ;
#7260 = DIRECTION ( 'NONE',  ( -0.2036417511401761582, -0.4895227362422917006, -0.8478782506317886769 ) ) ;
#7261 = CARTESIAN_POINT ( 'NONE',  ( -0.3267488823401686893, 0.1886891683789005680, -3.100567304031762284 ) ) ;
#7262 = CARTESIAN_POINT ( 'NONE',  ( -0.09139240964747710749, -0.07874015748031500117, -1.188614124534770567E-17 ) ) ;
#7263 = ADVANCED_FACE ( 'NONE', ( #5319 ), #9949, .F. ) ;
#7264 = ORIENTED_EDGE ( 'NONE', *, *, #12244, .T. ) ;
#7265 = CARTESIAN_POINT ( 'NONE',  ( -9.069736220472442904E-16, -0.8267716535433071723, 0.000000000000000000 ) ) ;
#7266 = VECTOR ( 'NONE', #3866, 39.37007874015748143 ) ;
#7267 = ADVANCED_FACE ( 'NONE', ( #668 ), #23367, .T. ) ;
#7268 = B_SPLINE_CURVE_WITH_KNOTS ( 'NONE', 3,
 ( #22288, #7180, #2780, #4774, #24268, #22021, #2921, #19760, #9014, #551 ),
 .UNSPECIFIED., .F., .F.,
 ( 4, 2, 2, 2, 4 ),
 ( 0.000000000000000000, 0.2500000000000000000, 0.5000000000000000000, 0.7500000000000000000, 1.000000000000000000 ),
 .UNSPECIFIED. ) ;
#7269 = CIRCLE ( 'NONE', #23083, 0.3126261861498082495 ) ;
#7270 = CARTESIAN_POINT ( 'NONE',  ( -0.0006615832605804723319, 0.6212594902576319411, 0.2574803149606298969 ) ) ;
#7271 = VERTEX_POINT ( 'NONE', #10709 ) ;
#7272 = ORIENTED_EDGE ( 'NONE', *, *, #11101, .F. ) ;
#7273 = VERTEX_POINT ( 'NONE', #10850 ) ;
#7274 = CARTESIAN_POINT ( 'NONE',  ( 0.4684132450478840082, -0.1062614382955253955, 0.2529987172365008030 ) ) ;
#7275 = CARTESIAN_POINT ( 'NONE',  ( 0.4620608682196346573, 0.08206165078060492779, 0.1992125984251968684 ) ) ;
#7276 = CARTESIAN_POINT ( 'NONE',  ( 0.3855916753051394363, 0.3382184156732163660, 1.747047244094488194 ) ) ;
#7277 = CARTESIAN_POINT ( 'NONE',  ( 0.3998447049182496382, 0.4754871227240771714, 0.09685039370078740717 ) ) ;
#7278 = EDGE_CURVE ( 'NONE', #20882, #14762, #16087, .T. ) ;
#7279 = ORIENTED_EDGE ( 'NONE', *, *, #19009, .T. ) ;
#7280 = CARTESIAN_POINT ( 'NONE',  ( -0.3740848232703756771, 0.04928467685643712209, -3.100567304031759175 ) ) ;
#7281 = CARTESIAN_POINT ( 'NONE',  ( 0.000000000000000000, 0.000000000000000000, 0.09685039370078740717 ) ) ;
#7282 = VERTEX_POINT ( 'NONE', #19743 ) ;
#7283 = CARTESIAN_POINT ( 'NONE',  ( -0.7874015748031496509, 0.3943205132762559462, -0.07664873632799094894 ) ) ;
#7284 = CARTESIAN_POINT ( 'NONE',  ( -0.3334645669291338987, 5.862181871850394349E-06, -1.869015748010449007 ) ) ;
#7285 = ORIENTED_EDGE ( 'NONE', *, *, #11966, .F. ) ;
#7286 = ORIENTED_EDGE ( 'NONE', *, *, #19531, .T. ) ;
#7287 = AXIS2_PLACEMENT_3D ( 'NONE', #21523, #8657, #17280 ) ;
#7288 = FACE_OUTER_BOUND ( 'NONE', #19185, .T. ) ;
#7290 = EDGE_LOOP ( 'NONE', ( #6807, #8826, #25513, #2762, #3340 ) ) ;
#7289 = DIRECTION ( 'NONE',  ( 0.000000000000000000, 1.000000000000000000, 0.000000000000000000 ) ) ;
#7291 = CARTESIAN_POINT ( 'NONE',  ( 0.000000000000000000, 0.5007874015748031704, -3.278217716535432842E-17 ) ) ;
#7292 = ORIENTED_EDGE ( 'NONE', *, *, #18293, .F. ) ;
#7293 = EDGE_LOOP ( 'NONE', ( #10418, #11662, #26327, #25967 ) ) ;
#7294 = ORIENTED_EDGE ( 'NONE', *, *, #18218, .F. ) ;
#7295 = CARTESIAN_POINT ( 'NONE',  ( -0.6562077975700453258, 2.612916929133858441E-14, 0.2362204724409449064 ) ) ;
#7296 = CARTESIAN_POINT ( 'NONE',  ( -0.1786951194748074845, 0.7326758143698267611, -0.6802888381030000042 ) ) ;
#7297 = CARTESIAN_POINT ( 'NONE',  ( -0.04841158226283256288, 0.1968503937007874127, -3.209690007240762366 ) ) ;
#7298 = LINE ( 'NONE', #9261, #3497 ) ;
#7299 = CARTESIAN_POINT ( 'NONE',  ( -0.3937007874015748254, 4.966087413865251393E-17, 0.4488188976377953110 ) ) ;
#7300 = EDGE_CURVE ( 'NONE', #6574, #11007, #20770, .T. ) ;
#7301 = CARTESIAN_POINT ( 'NONE',  ( 0.3606190329934327310, 0.4297690281277732338, 0.07676968503937006694 ) ) ;
#7302 = CARTESIAN_POINT ( 'NONE',  ( 0.3998447049182889956, 0.4754871227240441423, 0.2574803149606298969 ) ) ;
#7303 = CARTESIAN_POINT ( 'NONE',  ( 0.02319089060378159983, 0.3543307086614173596, 1.953740157480315043 ) ) ;
#7304 = ADVANCED_FACE ( 'NONE', ( #2504 ), #18969, .T. ) ;
#7305 = VECTOR ( 'NONE', #20839, 39.37007874015748143 ) ;
#7306 = DIRECTION ( 'NONE',  ( -1.000000000000000000, 0.000000000000000000, 0.000000000000000000 ) ) ;
#7307 = AXIS2_PLACEMENT_3D ( 'NONE', #9577, #20051, #20188 ) ;
#7308 = DIRECTION ( 'NONE',  ( 0.000000000000000000, 0.000000000000000000, -1.000000000000000000 ) ) ;
#7309 = ADVANCED_FACE ( 'NONE', ( #25970 ), #19883, .T. ) ;
#7310 = CARTESIAN_POINT ( 'NONE',  ( -0.3988311005573134116, 0.4763376377694984454, 0.09685039370078740717 ) ) ;
#7311 = CARTESIAN_POINT ( 'NONE',  ( 0.000000000000000000, 0.000000000000000000, -0.01377952755905511792 ) ) ;
#7312 = CARTESIAN_POINT ( 'NONE',  ( -0.5314960629921260393, -0.03478633594543723700, 1.747047244094488194 ) ) ;
#7313 = FACE_OUTER_BOUND ( 'NONE', #13168, .T. ) ;
#7314 = ADVANCED_FACE ( 'NONE', ( #8998 ), #2359, .T. ) ;
#7315 = ORIENTED_EDGE ( 'NONE', *, *, #2449, .F. ) ;
#7316 = AXIS2_PLACEMENT_3D ( 'NONE', #16348, #706, #20055 ) ;
#7317 = CARTESIAN_POINT ( 'NONE',  ( 0.3986320731132085293, -0.2308081338369910029, 0.1639447408811634532 ) ) ;
#7318 = EDGE_LOOP ( 'NONE', ( #20741, #23290, #16224, #11357, #2992 ) ) ;
#7319 = FACE_OUTER_BOUND ( 'NONE', #20969, .T. ) ;
#7320 = ORIENTED_EDGE ( 'NONE', *, *, #18108, .T. ) ;
#7321 = CARTESIAN_POINT ( 'NONE',  ( 0.03937007874015747977, 0.3346456692913385988, 0.000000000000000000 ) ) ;
#7322 = ORIENTED_EDGE ( 'NONE', *, *, #2911, .T. ) ;
#7323 = CARTESIAN_POINT ( 'NONE',  ( -0.4669911931914798586, -0.1585706980422492696, -1.569881889763779625 ) ) ;
#7324 = CARTESIAN_POINT ( 'NONE',  ( -2.073220866141732523E-16, 0.07874015748031495954, 1.692913385826771533 ) ) ;
#7325 = ORIENTED_EDGE ( 'NONE', *, *, #16824, .F. ) ;
#7326 = CARTESIAN_POINT ( 'NONE',  ( -0.3362148458988341582, -0.4382482975805541692, 0.9399606299212598381 ) ) ;
#7327 = EDGE_LOOP ( 'NONE', ( #8306, #19358, #21764, #1544 ) ) ;
#7328 = ORIENTED_EDGE ( 'NONE', *, *, #13134, .F. ) ;
#7329 = DIRECTION ( 'NONE',  ( -1.000000000000000000, 0.000000000000000000, 0.000000000000000000 ) ) ;
#7330 = AXIS2_PLACEMENT_3D ( 'NONE', #5121, #26881, #16297 ) ;
#7331 = EDGE_CURVE ( 'NONE', #18692, #15200, #6622, .T. ) ;
#7332 = CARTESIAN_POINT ( 'NONE',  ( 0.6055690743987126590, -0.2581485381169802973, 0.4471263839182408883 ) ) ;
#7333 = AXIS2_PLACEMENT_3D ( 'NONE', #6724, #2732, #26199 ) ;
#7334 = CONTEXT_DEPENDENT_SHAPE_REPRESENTATION ( #27684, #18147 ) ;
#7335 = DIRECTION ( 'NONE',  ( 0.000000000000000000, 0.000000000000000000, -1.000000000000000000 ) ) ;
#7336 = LINE ( 'NONE', #11298, #16613 ) ;
#7337 = LINE ( 'NONE', #20334, #12740 ) ;
#7338 = DIRECTION ( 'NONE',  ( 0.000000000000000000, 0.000000000000000000, 1.000000000000000000 ) ) ;
#7339 = ADVANCED_FACE ( 'NONE', ( #23454 ), #23862, .T. ) ;
#7340 = CONICAL_SURFACE ( 'NONE', #1038, 0.3458446900868161200, 0.2407725888118960322 ) ;
#7341 = ADVANCED_FACE ( 'NONE', ( #17077 ), #25555, .F. ) ;
#7342 = CARTESIAN_POINT ( 'NONE',  ( -0.4133615125900214071, 0.4936731914959181511, 0.2359405056196126338 ) ) ;
#7343 = CARTESIAN_POINT ( 'NONE',  ( 0.1078280746903870629, -0.3175540113612215221, 1.953740157480315043 ) ) ;
#7344 = UNCERTAINTY_MEASURE_WITH_UNIT (LENGTH_MEASURE( 1.000000000000000082E-05 ), #9669, 'distance_accuracy_value', 'NONE') ;
#7345 = CYLINDRICAL_SURFACE ( 'NONE', #17731, 0.6212598425196850238 ) ;
#7346 = FACE_BOUND ( 'NONE', #6653, .T. ) ;
#7347 = CARTESIAN_POINT ( 'NONE',  ( -0.6513233937849554067, -0.01774504213867074409, 0.2362204724409449896 ) ) ;
#7348 = DIRECTION ( 'NONE',  ( 1.000000000000000000, 0.000000000000000000, 0.000000000000000000 ) ) ;
#7349 = DIRECTION ( 'NONE',  ( 0.000000000000000000, 0.000000000000000000, -1.000000000000000000 ) ) ;
#7350 = DIRECTION ( 'NONE',  ( 0.000000000000000000, 0.000000000000000000, 1.000000000000000000 ) ) ;
#7351 = PRODUCT_DEFINITION_SHAPE ( 'NONE', 'NONE',  #27905 ) ;
#7352 = DIRECTION ( 'NONE',  ( 0.000000000000000000, 0.000000000000000000, 1.000000000000000000 ) ) ;
#7353 = CARTESIAN_POINT ( 'NONE',  ( 0.6119360453657125554, 0.1072290460171897442, 0.09685039370078740717 ) ) ;
#7354 = CIRCLE ( 'NONE', #7805, 0.1673228346456692994 ) ;
#7355 = ORIENTED_EDGE ( 'NONE', *, *, #25408, .T. ) ;
#7356 = ORIENTED_EDGE ( 'NONE', *, *, #23911, .T. ) ;
#7357 = AXIS2_PLACEMENT_3D ( 'NONE', #26685, #22598, #20624 ) ;
#7358 = CARTESIAN_POINT ( 'NONE',  ( 3.606039370078740678E-16, -0.6299212598425196763, 0.000000000000000000 ) ) ;
#7359 = CARTESIAN_POINT ( 'NONE',  ( -0.2992781133269515892, -0.6197069291944330427, 0.3401574803149606252 ) ) ;
#7360 = ORIENTED_EDGE ( 'NONE', *, *, #1708, .T. ) ;
#7361 = ORIENTED_EDGE ( 'NONE', *, *, #22319, .T. ) ;
#7362 = DIRECTION ( 'NONE',  ( 0.000000000000000000, 0.000000000000000000, 1.000000000000000000 ) ) ;
#7363 = ORIENTED_EDGE ( 'NONE', *, *, #12786, .F. ) ;
#7364 = EDGE_CURVE ( 'NONE', #27472, #550, #4616, .T. ) ;
#7365 = CARTESIAN_POINT ( 'NONE',  ( 0.7873253891977465280, 0.2997731478012109485, -0.1260073171955472526 ) ) ;
#7366 = EDGE_CURVE ( 'NONE', #21655, #6603, #12661, .T. ) ;
#7367 = AXIS2_PLACEMENT_3D ( 'NONE', #6849, #15477, #4714 ) ;
#7368 = CIRCLE ( 'NONE', #4224, 0.2952755905264887182 ) ;
#7369 = DIRECTION ( 'NONE',  ( 0.000000000000000000, 0.000000000000000000, 1.000000000000000000 ) ) ;
#7370 = AXIS2_PLACEMENT_3D ( 'NONE', #26123, #20035, #6778 ) ;
#7371 = ORIENTED_EDGE ( 'NONE', *, *, #3867, .T. ) ;
#7372 = CARTESIAN_POINT ( 'NONE',  ( -0.2211428102655751127, -0.2521176338356575508, 1.973425196850393970 ) ) ;
#7373 = CARTESIAN_POINT ( 'NONE',  ( -0.4954415918535620134, 0.1327036767636087800, -1.550196850393700920 ) ) ;
#7374 = CARTESIAN_POINT ( 'NONE',  ( -0.5368353335967093187, 0.1442704874421232575, 0.9202755905511812440 ) ) ;
#7375 = AXIS2_PLACEMENT_3D ( 'NONE', #20025, #678, #9266 ) ;
#7376 = DIRECTION ( 'NONE',  ( 0.000000000000000000, 0.000000000000000000, -1.000000000000000000 ) ) ;
#7377 = DIRECTION ( 'NONE',  ( 0.000000000000000000, 0.000000000000000000, 1.000000000000000000 ) ) ;
#7378 = DIRECTION ( 'NONE',  ( 0.000000000000000000, -1.000000000000000000, 0.000000000000000000 ) ) ;
#7379 = CARTESIAN_POINT ( 'NONE',  ( -0.4423390553432505201, 0.2180862235769355506, -1.569881889763779625 ) ) ;
#7380 = FACE_OUTER_BOUND ( 'NONE', #25252, .T. ) ;
#7381 = CARTESIAN_POINT ( 'NONE',  ( 0.2990496115119744003, -0.6198172806990825956, 0.3401591245381555551 ) ) ;
#7382 = EDGE_CURVE ( 'NONE', #247, #1086, #6803, .T. ) ;
#7383 = CARTESIAN_POINT ( 'NONE',  ( 0.1669561253493014596, -0.4569961989609055975, 0.2467937633349458482 ) ) ;
#7384 = AXIS2_PLACEMENT_3D ( 'NONE', #10051, #16551, #7808 ) ;
#7385 = ORIENTED_EDGE ( 'NONE', *, *, #8608, .F. ) ;
#7386 = EDGE_CURVE ( 'NONE', #18758, #1231, #23938, .T. ) ;
#7387 = FACE_OUTER_BOUND ( 'NONE', #983, .T. ) ;
#7388 = EDGE_CURVE ( 'NONE', #15279, #15981, #489, .T. ) ;
#7389 = ORIENTED_EDGE ( 'NONE', *, *, #17516, .F. ) ;
#7390 = CARTESIAN_POINT ( 'NONE',  ( -0.7874015748031496509, 0.4828108945773819105, 0.1423708153504031348 ) ) ;
#7391 = VERTEX_POINT ( 'NONE', #2900 ) ;
#7392 = AXIS2_PLACEMENT_3D ( 'NONE', #7080, #11041, #13151 ) ;
#7393 = CARTESIAN_POINT ( 'NONE',  ( 0.2761764805255846333, -0.3599896729929844552, -1.934055118110236338 ) ) ;
#7394 = CARTESIAN_POINT ( 'NONE',  ( 0.4149306118460625581, -0.2388850582578112280, 0.1920935997041153531 ) ) ;
#7395 = DIRECTION ( 'NONE',  ( 0.000000000000000000, 1.000000000000000000, 0.000000000000000000 ) ) ;
#7396 = DIRECTION ( 'NONE',  ( 0.000000000000000000, -1.000000000000000000, 0.000000000000000000 ) ) ;
#7397 = ADVANCED_FACE ( 'NONE', ( #5168, #20150 ), #11813, .T. ) ;
#7398 = EDGE_CURVE ( 'NONE', #8484, #2005, #13795, .T. ) ;
#7399 = AXIS2_PLACEMENT_3D ( 'NONE', #14661, #2998, #7396 ) ;
#7400 = DIRECTION ( 'NONE',  ( 0.000000000000000000, 0.000000000000000000, -1.000000000000000000 ) ) ;
#7401 = DIRECTION ( 'NONE',  ( 0.000000000000000000, 0.000000000000000000, -1.000000000000000000 ) ) ;
#7402 = ORIENTED_EDGE ( 'NONE', *, *, #9485, .F. ) ;
#7403 = CARTESIAN_POINT ( 'NONE',  ( -1.197070535079588716, 0.4724409448818898127, -1.197070535079588716 ) ) ;
#7404 = CARTESIAN_POINT ( 'NONE',  ( -0.4303639208847589437, -0.1153623459797714496, -1.934055118110236560 ) ) ;
#7405 = CARTESIAN_POINT ( 'NONE',  ( -0.3765118517642104257, 0.000000000000000000, -3.100567304031763172 ) ) ;
#7406 = CARTESIAN_POINT ( 'NONE',  ( 0.000000000000000000, 0.000000000000000000, 1.914370078775489148 ) ) ;
#7407 = CIRCLE ( 'NONE', #21421, 0.3584231247409862542 ) ;
#7408 = ORIENTED_EDGE ( 'NONE', *, *, #24538, .T. ) ;
#7409 = CARTESIAN_POINT ( 'NONE',  ( -0.4446020952038907681, -0.02909913904661340714, -1.934055118110236338 ) ) ;
#7410 = AXIS2_PLACEMENT_3D ( 'NONE', #26509, #2242, #15127 ) ;
#7411 = CIRCLE ( 'NONE', #27268, 0.7874015748031496509 ) ;
#7412 = CARTESIAN_POINT ( 'NONE',  ( 0.5744851493189444547, 0.4591414886171028553, 0.2763636194376414279 ) ) ;
#7413 = DIRECTION ( 'NONE',  ( -0.2036417511401758251, -0.9790454724845842893, 0.000000000000000000 ) ) ;
#7414 = CARTESIAN_POINT ( 'NONE',  ( 0.3855916753051445989, -0.3382184156732112590, 1.766732283464566899 ) ) ;
#7415 = ORIENTED_EDGE ( 'NONE', *, *, #22856, .T. ) ;
#7416 = CARTESIAN_POINT ( 'NONE',  ( 0.000000000000000000, 0.000000000000000000, 0.2755905511811023723 ) ) ;
#7417 = CARTESIAN_POINT ( 'NONE',  ( -0.2836590635674511307, -0.2488091035917043836, -3.100567304031761395 ) ) ;
#7418 = CARTESIAN_POINT ( 'NONE',  ( -0.6094642026423211512, 1.111319899719084070, -0.06074667524627151011 ) ) ;
#7419 = CARTESIAN_POINT ( 'NONE',  ( -0.2070393714800602414, -0.1127906890684966662, 0.2362204724409449064 ) ) ;
#7420 = EDGE_CURVE ( 'NONE', #1231, #4752, #12190, .T. ) ;
#7421 = CIRCLE ( 'NONE', #18712, 0.4692913385826771866 ) ;
#7422 = CARTESIAN_POINT ( 'NONE',  ( 0.3239425792934414461, -0.08676778863010961573, 1.953740157480315043 ) ) ;
#7423 = VERTEX_POINT ( 'NONE', #20011 ) ;
#7424 = EDGE_LOOP ( 'NONE', ( #12107, #24798 ) ) ;
#7425 = ORIENTED_EDGE ( 'NONE', *, *, #24446, .F. ) ;
#7426 = CARTESIAN_POINT ( 'NONE',  ( -0.3528405259361242496, -0.7288848593461209058, -0.6846649188871202218 ) ) ;
#7427 = DIRECTION ( 'NONE',  ( 0.000000000000000000, 1.000000000000000000, 0.000000000000000000 ) ) ;
#7428 = ADVANCED_FACE ( 'NONE', ( #15782, #3181 ), #9397, .T. ) ;
#7429 = ORIENTED_EDGE ( 'NONE', *, *, #14472, .F. ) ;
#7430 = ORIENTED_EDGE ( 'NONE', *, *, #26186, .T. ) ;
#7431 = CARTESIAN_POINT ( 'NONE',  ( -0.6996199877990079141, 0.1591959485999228652, 0.2265176967194976465 ) ) ;
#7432 = CARTESIAN_POINT ( 'NONE',  ( 2.531258147843938596E-16, 0.3937007873309092409, 2.066929133858267598 ) ) ;
#7433 = CIRCLE ( 'NONE', #5674, 0.5007874015748031704 ) ;
#7434 = CYLINDRICAL_SURFACE ( 'NONE', #2715, 0.7500000000000001110 ) ;
#7435 = AXIS2_PLACEMENT_3D ( 'NONE', #21554, #26202, #17317 ) ;
#7436 = FACE_OUTER_BOUND ( 'NONE', #23100, .T. ) ;
#7437 = DIRECTION ( 'NONE',  ( 1.000000000000000000, 0.000000000000000000, 0.000000000000000000 ) ) ;
#7438 = CARTESIAN_POINT ( 'NONE',  ( 0.000000000000000000, 0.000000000000000000, 1.953740157480315043 ) ) ;
#7439 = PLANE ( 'NONE',  #25438 ) ;
#7440 = DIRECTION ( 'NONE',  ( 0.000000000000000000, 0.000000000000000000, 1.000000000000000000 ) ) ;
#7441 = CARTESIAN_POINT ( 'NONE',  ( -0.2161381151963043257, -0.2817310484609166221, 1.953740157480315043 ) ) ;
#7442 = CIRCLE ( 'NONE', #6572, 0.1299232283464566984 ) ;
#7443 = ORIENTED_EDGE ( 'NONE', *, *, #4318, .F. ) ;
#7444 = DIRECTION ( 'NONE',  ( 0.000000000000000000, 0.000000000000000000, -1.000000000000000000 ) ) ;
#7445 = CARTESIAN_POINT ( 'NONE',  ( 0.000000000000000000, 0.8267716535433071723, 0.4488188976377953110 ) ) ;
#7446 = ADVANCED_FACE ( 'NONE', ( #6893, #18001 ), #20432, .T. ) ;
#7447 = DIRECTION ( 'NONE',  ( 1.000000000000000000, 0.000000000000000000, 0.000000000000000000 ) ) ;
#7448 = DIRECTION ( 'NONE',  ( 0.000000000000000000, 0.000000000000000000, 1.000000000000000000 ) ) ;
#7449 = CARTESIAN_POINT ( 'NONE',  ( -0.2355331214654103611, -0.4777261797697372470, 1.747047244094488194 ) ) ;
#7450 = CARTESIAN_POINT ( 'NONE',  ( 0.3680051700917442714, 0.2263466406172266743, -0.3920438816715699493 ) ) ;
#7452 = EDGE_CURVE ( 'NONE', #18836, #19875, #27112, .T. ) ;
#7451 = TOROIDAL_SURFACE ( 'NONE', #2058, 0.6102362204724409711, 0.1299212598425196763 ) ;
#7453 = ORIENTED_EDGE ( 'NONE', *, *, #5230, .F. ) ;
#7454 = DIRECTION ( 'NONE',  ( 1.000000000000000000, 0.000000000000000000, 0.000000000000000000 ) ) ;
#7455 = VERTEX_POINT ( 'NONE', #15521 ) ;
#7456 = DIRECTION ( 'NONE',  ( 1.000000000000000000, 0.000000000000000000, 0.000000000000000000 ) ) ;
#7457 = SHAPE_REPRESENTATION_RELATIONSHIP ( 'NONE' , 'NONE' ,  #20013, #26510 ) ;
#7458 = EDGE_CURVE ( 'NONE', #7455, #4928, #5959, .T. ) ;
#7459 = VERTEX_POINT ( 'NONE', #7432 ) ;
#7460 = CARTESIAN_POINT ( 'NONE',  ( -0.01968503937007873988, 0.000000000000000000, 0.000000000000000000 ) ) ;
#7461 = ORIENTED_EDGE ( 'NONE', *, *, #7084, .T. ) ;
#7462 = ORIENTED_EDGE ( 'NONE', *, *, #8151, .F. ) ;
#7463 = B_SPLINE_CURVE_WITH_KNOTS ( 'NONE', 3,
 ( #15816, #26530, #26677, #9436 ),
 .UNSPECIFIED., .F., .F.,
 ( 4, 4 ),
 ( 0.3125269569790670721, 0.3142031952238389936 ),
 .UNSPECIFIED. ) ;
#7464 = CARTESIAN_POINT ( 'NONE',  ( -0.4763861460130329739, 0.1275996891957754675, -1.569881889763779625 ) ) ;
#7465 = ORIENTED_EDGE ( 'NONE', *, *, #15595, .F. ) ;
#7466 = CARTESIAN_POINT ( 'NONE',  ( -0.2860899518037490763, 0.4954156765914824456, 0.9399606299212598381 ) ) ;
#7467 = EDGE_LOOP ( 'NONE', ( #24320, #21051, #7570, #16923 ) ) ;
#7468 = EDGE_CURVE ( 'NONE', #550, #6621, #16061, .T. ) ;
#7469 = ORIENTED_EDGE ( 'NONE', *, *, #4961, .T. ) ;
#7470 = AXIS2_PLACEMENT_3D ( 'NONE', #26049, #6708, #21959 ) ;
#7471 = CARTESIAN_POINT ( 'NONE',  ( -2.185478346456693112E-16, 0.8162224727389330026, 1.006043748880834642E-16 ) ) ;
#7472 = CARTESIAN_POINT ( 'NONE',  ( 0.2230788859036007821, 0.2650812153444456754, 0.1276989850664093651 ) ) ;
#7473 = DIRECTION ( 'NONE',  ( 0.000000000000000000, 1.000000000000000000, 0.000000000000000000 ) ) ;
#7474 = FACE_OUTER_BOUND ( 'NONE', #18850, .T. ) ;
#7475 = CARTESIAN_POINT ( 'NONE',  ( -2.073220866141732523E-16, 0.07874015748031491790, 1.692913385826771533 ) ) ;
#7476 = CARTESIAN_POINT ( 'NONE',  ( -0.4359497604187455022, 0.3683017918443335925, 0.1859854795144792461 ) ) ;
#7477 = DIRECTION ( 'NONE',  ( 0.000000000000000000, 0.000000000000000000, -1.000000000000000000 ) ) ;
#7478 = B_SPLINE_CURVE_WITH_KNOTS ( 'NONE', 3,
 ( #21464, #16801, #14567, #12968, #3945, #14712, #1961, #6350, #23593, #36 ),
 .UNSPECIFIED., .F., .F.,
 ( 4, 2, 2, 2, 4 ),
 ( 0.000000000000000000, 0.2500000000000001665, 0.5000000000000003331, 0.7500000000000001110, 1.000000000000000000 ),
 .UNSPECIFIED. ) ;
#7479 = EDGE_CURVE ( 'NONE', #10528, #23039, #19417, .T. ) ;
#7480 = CARTESIAN_POINT ( 'NONE',  ( -0.4068047116056149881, 0.4858504993699251928, 0.1061598535658933862 ) ) ;
#7481 = CARTESIAN_POINT ( 'NONE',  ( -0.2660793235464293804, -0.2041304421298503202, 1.953740157480315043 ) ) ;
#7482 = VERTEX_POINT ( 'NONE', #3318 ) ;
#7483 = CARTESIAN_POINT ( 'NONE',  ( 0.000000000000000000, 0.000000000000000000, 0.4724409448818898127 ) ) ;
#7484 = CARTESIAN_POINT ( 'NONE',  ( 0.1522836969735573143, 0.4909267390297480382, -0.05591742528025173131 ) ) ;
#7485 = AXIS2_PLACEMENT_3D ( 'NONE', #10802, #4309, #25782 ) ;
#7486 = CARTESIAN_POINT ( 'NONE',  ( -0.6102864789886656149, -0.1643143352007618574, 0.2257035431949488136 ) ) ;
#7487 = DIRECTION ( 'NONE',  ( -0.000000000000000000, -1.000000000000000000, -0.000000000000000000 ) ) ;
#7488 = CARTESIAN_POINT ( 'NONE',  ( 0.6106000000000000316, -0.09842519683305382683, 0.000000000000000000 ) ) ;
#7489 = CARTESIAN_POINT ( 'NONE',  ( 0.1318897637674583401, 1.615183770381184452E-17, -4.330708661396418080 ) ) ;
#7490 = CARTESIAN_POINT ( 'NONE',  ( -0.2131049448084480213, -0.5835666837866708700, 0.2574803149606298969 ) ) ;
#7491 = EDGE_CURVE ( 'NONE', #24053, #26265, #10399, .T. ) ;
#7492 = VERTEX_POINT ( 'NONE', #16612 ) ;
#7493 = ADVANCED_FACE ( 'NONE', ( #18859 ), #15804, .T. ) ;
#7494 = VERTEX_POINT ( 'NONE', #12093 ) ;
#7495 = ORIENTED_EDGE ( 'NONE', *, *, #15197, .T. ) ;
#7496 = CARTESIAN_POINT ( 'NONE',  ( 0.1447526197146039584, -0.3977045540727763839, 0.1377952755905511861 ) ) ;
#7497 = AXIS2_PLACEMENT_3D ( 'NONE', #22749, #18351, #12293 ) ;
#7498 = FACE_OUTER_BOUND ( 'NONE', #17488, .T. ) ;
#7499 = CARTESIAN_POINT ( 'NONE',  ( 0.07870736599822267254, 0.2165354330708661457, -3.608715228723538893 ) ) ;
#7500 = ORIENTED_EDGE ( 'NONE', *, *, #26466, .F. ) ;
#7501 = DIRECTION ( 'NONE',  ( 0.000000000000000000, 0.7071067805519554161, 0.7071067818211396183 ) ) ;
#7502 = CARTESIAN_POINT ( 'NONE',  ( -0.09139240964747702423, 0.07874015748031500117, -1.981023540891279271E-18 ) ) ;
#7503 = ORIENTED_EDGE ( 'NONE', *, *, #18790, .T. ) ;
#7504 = CIRCLE ( 'NONE', #11550, 0.09842519685039370636 ) ;
#7505 = B_SPLINE_CURVE_WITH_KNOTS ( 'NONE', 3,
 ( #548, #6911, #23736, #20030, #11139, #21612, #19757, #15534 ),
 .UNSPECIFIED., .F., .F.,
 ( 4, 2, 2, 4 ),
 ( 0.000000000000000000, 0.1249999999999998335, 0.2499999999999997780, 0.5000000000000000000 ),
 .UNSPECIFIED. ) ;
#7506 = DIRECTION ( 'NONE',  ( -1.000000000000000000, 0.000000000000000000, 0.000000000000000000 ) ) ;
#7507 = CARTESIAN_POINT ( 'NONE',  ( 0.6175000359513720394, 0.6841573636653760504, -0.3528259788121539398 ) ) ;
#7508 = ADVANCED_FACE ( 'NONE', ( #26936, #11959 ), #7728, .T. ) ;
#7509 = DIRECTION ( 'NONE',  ( -1.000000000000000000, 0.000000000000000000, 0.000000000000000000 ) ) ;
#7510 = CARTESIAN_POINT ( 'NONE',  ( 2.632951206231566310, -0.4724409448818898127, 0.9491381768041928790 ) ) ;
#7511 = EDGE_LOOP ( 'NONE', ( #6161, #22048, #13340 ) ) ;
#7512 = ORIENTED_EDGE ( 'NONE', *, *, #6931, .F. ) ;
#7513 = DIRECTION ( 'NONE',  ( 0.000000000000000000, 0.000000000000000000, 1.000000000000000000 ) ) ;
#7514 = CARTESIAN_POINT ( 'NONE',  ( -0.4600326175569863785, 0.2268096725200117181, -1.550196850393700920 ) ) ;
#7515 = FACE_OUTER_BOUND ( 'NONE', #21445, .T. ) ;
#7516 = PRODUCT_DEFINITION_FORMATION_WITH_SPECIFIED_SOURCE ( 'ANY', '', #2147, .NOT_KNOWN. ) ;
#7517 = CARTESIAN_POINT ( 'NONE',  ( -0.2442565704126265502, 0.4954197419817717996, 0.9399606299212598381 ) ) ;
#7518 = DIRECTION ( 'NONE',  ( 1.000000000000000000, 0.000000000000000000, 0.000000000000000000 ) ) ;
#7519 = AXIS2_PLACEMENT_3D ( 'NONE', #23815, #6718, #4584 ) ;
#7520 = FACE_OUTER_BOUND ( 'NONE', #221, .T. ) ;
#7521 = ORIENTED_EDGE ( 'NONE', *, *, #25217, .T. ) ;
#7522 = DIRECTION ( 'NONE',  ( 1.000000000000000000, 0.000000000000000000, 0.000000000000000000 ) ) ;
#7523 = CARTESIAN_POINT ( 'NONE',  ( 0.3252100150720242944, 0.3707612262533179215, -1.569881889763779625 ) ) ;
#7524 = SURFACE_STYLE_USAGE ( .BOTH. , #1312 ) ;
#7525 = CIRCLE ( 'NONE', #9842, 0.3771653543307086909 ) ;
#7526 = FACE_BOUND ( 'NONE', #21577, .T. ) ;
#7527 = CARTESIAN_POINT ( 'NONE',  ( -0.4157391792961063204, 0.3323952789219086768, 0.1322834645669291320 ) ) ;
#7528 = DIRECTION ( 'NONE',  ( -0.5000000000000002220, -0.8660254037844384856, 0.000000000000000000 ) ) ;
#7529 = DIRECTION ( 'NONE',  ( 1.000000000000000000, 0.000000000000000000, 0.000000000000000000 ) ) ;
#7530 = ADVANCED_FACE ( 'NONE', ( #18431 ), #12518, .F. ) ;
#7531 = ORIENTED_EDGE ( 'NONE', *, *, #967, .T. ) ;
#7532 = CYLINDRICAL_SURFACE ( 'NONE', #3901, 0.3346456692913385988 ) ;
#7533 = DIRECTION ( 'NONE',  ( 0.000000000000000000, 0.000000000000000000, -1.000000000000000000 ) ) ;
#7534 = VERTEX_POINT ( 'NONE', #21134 ) ;
#7535 = CARTESIAN_POINT ( 'NONE',  ( -0.0005189969344232283309, 0.3771649972486724733, 0.07637795275590551769 ) ) ;
#7536 = ORIENTED_EDGE ( 'NONE', *, *, #11302, .F. ) ;
#7537 = CARTESIAN_POINT ( 'NONE',  ( -0.4149306118455106107, -0.2388850582574924275, 0.1920935997045936094 ) ) ;
#7538 = CARTESIAN_POINT ( 'NONE',  ( -0.1601448837025137850, -0.4411213145380133982, 0.1992142434433712694 ) ) ;
#7539 = DIRECTION ( 'NONE',  ( 1.000000000000000000, 0.000000000000000000, 0.000000000000000000 ) ) ;
#7540 = CIRCLE ( 'NONE', #17030, 0.6193720790381457286 ) ;
#7541 = CARTESIAN_POINT ( 'NONE',  ( -0.07874015748031495954, 0.000000000000000000, 0.000000000000000000 ) ) ;
#7542 = DIRECTION ( 'NONE',  ( 0.000000000000000000, 1.000000000000000000, 0.000000000000000000 ) ) ;
#7543 = ORIENTED_EDGE ( 'NONE', *, *, #3094, .T. ) ;
#7544 = DIRECTION ( 'NONE',  ( 0.000000000000000000, 0.000000000000000000, -1.000000000000000000 ) ) ;
#7545 = DIRECTION ( 'NONE',  ( 1.000000000000000000, 0.000000000000000000, 0.000000000000000000 ) ) ;
#7546 = VERTEX_POINT ( 'NONE', #7575 ) ;
#7547 = CARTESIAN_POINT ( 'NONE',  ( -0.3765118517642104257, 0.000000000000000000, -3.100567304031763172 ) ) ;
#7548 = DIRECTION ( 'NONE',  ( 0.000000000000000000, 1.000000000000000000, 0.000000000000000000 ) ) ;
#7549 = CARTESIAN_POINT ( 'NONE',  ( 0.000000000000000000, 0.6881889763779527325, 0.1322810039474933141 ) ) ;
#7550 = ORIENTED_EDGE ( 'NONE', *, *, #7382, .T. ) ;
#7551 = EDGE_CURVE ( 'NONE', #6711, #17345, #15394, .T. ) ;
#7552 = CARTESIAN_POINT ( 'NONE',  ( -0.4527559054764770385, 0.02963280468031418563, -1.934055118110236338 ) ) ;
#7553 = AXIS2_PLACEMENT_3D ( 'NONE', #10459, #4117, #5821 ) ;
#7554 = PRODUCT_CONTEXT ( 'NONE', #24400, 'mechanical' ) ;
#7555 = ORIENTED_EDGE ( 'NONE', *, *, #15537, .F. ) ;
#7556 = EDGE_CURVE ( 'NONE', #25001, #607, #1835, .T. ) ;
#7557 = AXIS2_PLACEMENT_3D ( 'NONE', #8907, #19925, #19789 ) ;
#7558 = AXIS2_PLACEMENT_3D ( 'NONE', #8425, #17316, #19581 ) ;
#7559 = CARTESIAN_POINT ( 'NONE',  ( -0.4101012214746874163, -0.6863629600575589240, -0.3597087265456967997 ) ) ;
#7560 = CARTESIAN_POINT ( 'NONE',  ( 0.1649135259617203753, -0.4856708409200670151, 1.747047244094488194 ) ) ;
#7561 = ORIENTED_EDGE ( 'NONE', *, *, #20852, .T. ) ;
#7562 = DIRECTION ( 'NONE',  ( 0.000000000000000000, 0.000000000000000000, -1.000000000000000000 ) ) ;
#7563 = CARTESIAN_POINT ( 'NONE',  ( 0.2296683860596776539, 0.2993674444872277962, -3.100567304031764060 ) ) ;
#7564 = CARTESIAN_POINT ( 'NONE',  ( 0.7874015748031496509, 0.2962865104657910753, -0.1276405476038844355 ) ) ;
#7565 = DIRECTION ( 'NONE',  ( 0.000000000000000000, 1.000000000000000000, 0.000000000000000000 ) ) ;
#7566 = ORIENTED_EDGE ( 'NONE', *, *, #15556, .F. ) ;
#7567 = CARTESIAN_POINT ( 'NONE',  ( -0.03359157810797404331, 0.5118124425185099913, -1.550196850393700920 ) ) ;
#7568 = CARTESIAN_POINT ( 'NONE',  ( 0.1288360683667812978, -0.3544784926413480086, 0.1992150590373740204 ) ) ;
#7569 = CARTESIAN_POINT ( 'NONE',  ( 0.0003454908279975884623, 0.3771652360013086902, 0.1992142436757342316 ) ) ;
#7570 = ORIENTED_EDGE ( 'NONE', *, *, #18019, .F. ) ;
#7571 = CARTESIAN_POINT ( 'NONE',  ( 0.05819755867303724045, 0.4417361510194101615, -1.934055118110236338 ) ) ;
#7572 = ORIENTED_EDGE ( 'NONE', *, *, #807, .T. ) ;
#7573 = ORIENTED_EDGE ( 'NONE', *, *, #4152, .F. ) ;
#7574 = CARTESIAN_POINT ( 'NONE',  ( -1.928513779527558736E-17, 0.000000000000000000, -0.02362204724409448786 ) ) ;
#7575 = CARTESIAN_POINT ( 'NONE',  ( 0.6707652279343464530, -0.1538768215239712522, 0.1322834645669291320 ) ) ;
#7576 = AXIS2_PLACEMENT_3D ( 'NONE', #25558, #8329, #10284 ) ;
#7577 = EDGE_CURVE ( 'NONE', #218, #4135, #21242, .T. ) ;
#7578 = VECTOR ( 'NONE', #3479, 39.37007874015748143 ) ;
#7579 = CARTESIAN_POINT ( 'NONE',  ( -0.03794311743615354227, 1.003836633634893838, -0.2033123174402287625 ) ) ;
#7580 = DIRECTION ( 'NONE',  ( -1.000000000000000000, 0.000000000000000000, 0.000000000000000000 ) ) ;
#7581 = TOROIDAL_SURFACE ( 'NONE', #25635, 0.8031496062992127261, 0.02362204724409448786 ) ;
#7582 = CARTESIAN_POINT ( 'NONE',  ( -0.5905511811023621549, 0.9448818897637796255, -1.639108661417322569E-17 ) ) ;
#7583 = CARTESIAN_POINT ( 'NONE',  ( 0.5979250048013408092, 0.9208089262530376740, -0.1508331457611719051 ) ) ;
#7584 = CARTESIAN_POINT ( 'NONE',  ( -4.821283464566928349E-18, 0.000000000000000000, -0.3779527559055118058 ) ) ;
#7585 = PRODUCT_DEFINITION_SHAPE ( 'NONE', 'NONE',  #27922 ) ;
#7586 = EDGE_CURVE ( 'NONE', #26351, #1498, #17633, .T. ) ;
#7587 = CARTESIAN_POINT ( 'NONE',  ( -0.06048688188729484105, 0.2165354330708661457, -3.193930428897817198 ) ) ;
#7588 = CARTESIAN_POINT ( 'NONE',  ( 0.1522836969735573143, 0.1970374587079574968, -0.4531137400369417145 ) ) ;
#7589 = PRODUCT_DEFINITION ( 'UNKNOWN', '', #7516, #27757 ) ;
#7591 = CARTESIAN_POINT ( 'NONE',  ( -0.3362336590883612808, 0.1141709026133623794, 1.953740157480315043 ) ) ;
#7590 = VECTOR ( 'NONE', #24721, 39.37007874015748143 ) ;
#7592 = EDGE_CURVE ( 'NONE', #23745, #10570, #24386, .T. ) ;
#7593 = ORIENTED_EDGE ( 'NONE', *, *, #27111, .F. ) ;
#7594 = SPHERICAL_SURFACE ( 'NONE', #14266, 0.07677362204724409722 ) ;
#7595 = CARTESIAN_POINT ( 'NONE',  ( -0.3361738726636556707, -1.237811886721866372, -0.6855454509606260238 ) ) ;
#7596 = FACE_OUTER_BOUND ( 'NONE', #17849, .T. ) ;
#7597 = ORIENTED_EDGE ( 'NONE', *, *, #7479, .T. ) ;
#7598 = EDGE_CURVE ( 'NONE', #20206, #24827, #3605, .T. ) ;
#7599 = B_SPLINE_CURVE_WITH_KNOTS ( 'NONE', 3,
 ( #7277, #12079, #19130, #20833, #12219, #27482 ),
 .UNSPECIFIED., .F., .F.,
 ( 4, 2, 4 ),
 ( 0.3108507187342950395, 0.3125269569790680158, 0.3142031952238389936 ),
 .UNSPECIFIED. ) ;
#7600 = CARTESIAN_POINT ( 'NONE',  ( 0.5949363243629232079, -0.1357903337134992172, 0.2362204724409449064 ) ) ;
#7601 = CARTESIAN_POINT ( 'NONE',  ( 0.1327036767659768302, -0.4954415918531079877, 1.747047244094488194 ) ) ;
#7602 = CARTESIAN_POINT ( 'NONE',  ( 0.000000000000000000, 0.4692913385826771866, 0.2374015748031496065 ) ) ;
#7603 = CARTESIAN_POINT ( 'NONE',  ( 0.3121994997598600552, -0.4069448477555897004, 1.766732283464566899 ) ) ;
#7604 = AXIS2_PLACEMENT_3D ( 'NONE', #5645, #22882, #3800 ) ;
#7605 = EDGE_LOOP ( 'NONE', ( #1814, #24887, #23706, #4426 ) ) ;
#7606 = VECTOR ( 'NONE', #2138, 39.37007874015748143 ) ;
#7607 = DIRECTION ( 'NONE',  ( 0.000000000000000000, 1.224646799147353700E-16, 1.000000000000000000 ) ) ;
#7608 = ORIENTED_EDGE ( 'NONE', *, *, #17689, .T. ) ;
#7609 = DIRECTION ( 'NONE',  ( 0.9749279121818235083, -0.2225209339563150035, 0.000000000000000000 ) ) ;
#7610 = SHAPE_REPRESENTATION_RELATIONSHIP ( 'NONE' , 'NONE' ,  #24703, #14395 ) ;
#7611 = CARTESIAN_POINT ( 'NONE',  ( -0.3858397471888794783, 0.2228126397720086582, -1.934055118110236338 ) ) ;
#7612 = DIRECTION ( 'NONE',  ( -1.000000000000000000, 0.000000000000000000, 0.000000000000000000 ) ) ;
#7613 = FACE_BOUND ( 'NONE', #22127, .T. ) ;
#7614 = EDGE_LOOP ( 'NONE', ( #18759, #18029 ) ) ;
#7615 = VERTEX_POINT ( 'NONE', #27080 ) ;
#7616 = CARTESIAN_POINT ( 'NONE',  ( -0.4423390553432507977, -0.2180862235769348567, -1.569881889763779625 ) ) ;
#7617 = CARTESIAN_POINT ( 'NONE',  ( 0.4334967711386992772, -0.2507361369899905879, 0.09684874903502814492 ) ) ;
#7618 = AXIS2_PLACEMENT_3D ( 'NONE', #20287, #5596, #13787 ) ;
#7619 = EDGE_LOOP ( 'NONE', ( #13085, #3377 ) ) ;
#7620 = ORIENTED_EDGE ( 'NONE', *, *, #296, .F. ) ;
#7621 = DIRECTION ( 'NONE',  ( 0.000000000000000000, 1.000000000000000000, 0.000000000000000000 ) ) ;
#7622 = CONTEXT_DEPENDENT_SHAPE_REPRESENTATION ( #19549, #4625 ) ;
#7623 = DIRECTION ( 'NONE',  ( 0.000000000000000000, 0.000000000000000000, 1.000000000000000000 ) ) ;
#7624 = LINE ( 'NONE', #9164, #386 ) ;
#7625 = CYLINDRICAL_SURFACE ( 'NONE', #2813, 0.8267716535433071723 ) ;
#7626 = AXIS2_PLACEMENT_3D ( 'NONE', #8424, #17044, #21423 ) ;
#7627 = EDGE_CURVE ( 'NONE', #6066, #24915, #19437, .T. ) ;
#7628 = CARTESIAN_POINT ( 'NONE',  ( -0.3988311005573134116, 0.4763376377694984454, 0.09685039370078740717 ) ) ;
#7629 = AXIS2_PLACEMENT_3D ( 'NONE', #22568, #14093, #7308 ) ;
#7630 = CARTESIAN_POINT ( 'NONE',  ( 0.04380447413658805633, -0.3324885138898231451, 1.953740157480315043 ) ) ;
#7631 = ADVANCED_FACE ( 'NONE', ( #9971, #18571 ), #20715, .T. ) ;
#7632 = VERTEX_POINT ( 'NONE', #1501 ) ;
#7633 = DIRECTION ( 'NONE',  ( 1.000000000000000000, 0.000000000000000000, 0.000000000000000000 ) ) ;
#7634 = LINE ( 'NONE', #5372, #27256 ) ;
#7635 = DIRECTION ( 'NONE',  ( 0.000000000000000000, 0.000000000000000000, 1.000000000000000000 ) ) ;
#7636 = CARTESIAN_POINT ( 'NONE',  ( 0.000000000000000000, 0.2273032555864669124, 9.010881889763779798E-17 ) ) ;
#7637 = DIRECTION ( 'NONE',  ( 0.000000000000000000, 0.000000000000000000, 1.000000000000000000 ) ) ;
#7638 = CARTESIAN_POINT ( 'NONE',  ( 0.5869493968219645641, 0.2133897621573070669, -0.3696019098714952711 ) ) ;
#7639 = CARTESIAN_POINT ( 'NONE',  ( -0.5905511811023621549, -0.4724409448818898127, -0.6411263657805729155 ) ) ;
#7640 = VERTEX_POINT ( 'NONE', #10111 ) ;
#7641 = ADVANCED_FACE ( 'NONE', ( #18723 ), #27360, .F. ) ;
#7642 = EDGE_LOOP ( 'NONE', ( #23460, #10976, #22405, #2092 ) ) ;
#7643 = VECTOR ( 'NONE', #14343, 39.37007874015748143 ) ;
#7644 = CARTESIAN_POINT ( 'NONE',  ( -0.07874015748031495954, 0.04546065111729338803, -0.3779527559055118058 ) ) ;
#7645 = CARTESIAN_POINT ( 'NONE',  ( -0.3218523081044682987, -0.6665164569857464638, 0.2161412452743130541 ) ) ;
#7646 = ORIENTED_EDGE ( 'NONE', *, *, #15688, .T. ) ;
#7647 = CARTESIAN_POINT ( 'NONE',  ( -0.4442189740295497402, 0.2564173815260738509, -1.550196850393700920 ) ) ;
#7648 = CARTESIAN_POINT ( 'NONE',  ( 0.6140435224042697371, 0.000000000000000000, 0.000000000000000000 ) ) ;
#7649 = B_SPLINE_CURVE_WITH_KNOTS ( 'NONE', 3,
 ( #15484, #13342, #21968, #22100, #26463, #7125 ),
 .UNSPECIFIED., .F., .F.,
 ( 4, 2, 4 ),
 ( 0.000000000000000000, 0.2500000000000000000, 0.5000000000000000000 ),
 .UNSPECIFIED. ) ;
#7650 = EDGE_LOOP ( 'NONE', ( #7655, #24551, #18992, #5554 ) ) ;
#7651 = CARTESIAN_POINT ( 'NONE',  ( -0.3412792617076849111, 0.05967164814832635888, 0.1377952755905512139 ) ) ;
#7652 = PLANE ( 'NONE',  #12275 ) ;
#7653 = EDGE_CURVE ( 'NONE', #2049, #5851, #21257, .T. ) ;
#7654 = CARTESIAN_POINT ( 'NONE',  ( -0.5811930530674194184, -0.4724394499398544278, -0.9954595798869386725 ) ) ;
#7655 = ORIENTED_EDGE ( 'NONE', *, *, #22554, .T. ) ;
#7656 = CARTESIAN_POINT ( 'NONE',  ( -0.03937007874015747977, -0.5905511811023621549, 7.232166136696967594E-17 ) ) ;
#7657 = ADVANCED_FACE ( 'NONE', ( #6582 ), #17208, .F. ) ;
#7658 = CARTESIAN_POINT ( 'NONE',  ( 0.3381512095065888901, -0.3856568748492107401, -1.550196850393700920 ) ) ;
#7659 = ORIENTED_EDGE ( 'NONE', *, *, #17985, .T. ) ;
#7660 = CARTESIAN_POINT ( 'NONE',  ( 0.2904160862623631489, 0.1677079028045434517, 1.973425196850393970 ) ) ;
#7661 = ADVANCED_FACE ( 'NONE', ( #27645 ), #15208, .T. ) ;
#7662 = VECTOR ( 'NONE', #19254, 39.37007874015748143 ) ;
#7663 = CARTESIAN_POINT ( 'NONE',  ( -0.1442704874421230077, 0.5368353335967094297, 0.9202755905511812440 ) ) ;
#7664 = B_SPLINE_CURVE_WITH_KNOTS ( 'NONE', 3,
 ( #18134, #17995, #18283, #13930, #9532, #20707, #7426, #3174, #16468, #26634, #14364, #1087, #11664, #16053, #1354, #24511, #25081, #5161, #5747, #14074, #11150, #16196, #9827, #24796, #3311, #11953, #20572, #1226, #3893, #12367, #18851, #3598, #10383, #27351, #10523, #2051, #14937, #15071, #25787, #23118, #19002, #27636, #21412, #14803, #25218, #27775, #6301, #10662, #8004, #8281, #3748, #20843, #16900, #16605, #19285, #25510, #8553, #9311, #6175, #19142, #8143, #12227, #21129, #17173, #12649, #1493, #20986, #25648, #5889, #8416, #14515, #1632, #23546, #17037, #25363, #23409, #6025, #21276, #4041, #6437, #4180, #10237 ),
 .UNSPECIFIED., .F., .F.,
 ( 4, 2, 2, 2, 1, 1, 1, 1, 2, 2, 2, 2, 2, 1, 1, 1, 2, 2, 2, 2, 2, 1, 1, 2, 2, 2, 1, 1, 1, 2, 2, 2, 1, 1, 1, 1, 2, 2, 1, 1, 1, 1, 1, 2, 2, 2, 2, 1, 1, 1, 2, 2, 4 ),
 ( 0.000000000000000000, 0.1250000000000016098, 0.1875000000000022482, 0.2187500000000024702, 0.2343750000000026090, 0.2421875000000024980, 0.2460937500000025258, 0.2480468750000025258, 0.2490234375000025813, 0.2500000000000026090, 0.3750000000000124900, 0.4375000000000175415, 0.4687500000000200395, 0.4843750000000213163, 0.4921875000000219824, 0.4960937500000222600, 0.4980468750000223155, 0.5000000000000223155, 0.6250000000000152101, 0.6875000000000116573, 0.7187500000000097700, 0.7343750000000088818, 0.7421875000000084377, 0.7460937500000082157, 0.7500000000000078826, 0.7812500000000063283, 0.7968750000000054401, 0.8046875000000049960, 0.8085937500000048850, 0.8105468750000047740, 0.8125000000000046629, 0.8437500000000036637, 0.8593750000000031086, 0.8671875000000028866, 0.8710937500000026645, 0.8730468750000025535, 0.8740234375000025535, 0.8750000000000025535, 0.8906250000000015543, 0.8984375000000009992, 0.9023437500000007772, 0.9042968750000006661, 0.9052734375000005551, 0.9057617187500005551, 0.9062500000000005551, 0.9218749999999998890, 0.9296874999999995559, 0.9335937499999993339, 0.9355468749999994449, 0.9365234374999994449, 0.9370117187499994449, 0.9374999999999994449, 1.000000000000000000 ),
 .UNSPECIFIED. ) ;
#7665 = AXIS2_PLACEMENT_3D ( 'NONE', #8427, #19153, #21555 ) ;
#7666 = DIRECTION ( 'NONE',  ( 0.000000000000000000, 1.000000000000000000, 0.000000000000000000 ) ) ;
#7667 = ORIENTED_EDGE ( 'NONE', *, *, #20733, .T. ) ;
#7668 = DIRECTION ( 'NONE',  ( 0.000000000000000000, -7.180547322999999937E-06, -0.9999999999742198442 ) ) ;
#7669 = ADVANCED_FACE ( 'NONE', ( #17313, #23686 ), #12924, .F. ) ;
#7670 = CARTESIAN_POINT ( 'NONE',  ( 0.3912931228432083297, 0.3001918266902350307, -1.569881889763779625 ) ) ;
#7671 = CARTESIAN_POINT ( 'NONE',  ( 0.1520643344662694629, -0.4930463976998556430, 0.03726710077533004067 ) ) ;
#7672 = AXIS2_PLACEMENT_3D ( 'NONE', #6107, #14741, #18786 ) ;
#7673 = VERTEX_POINT ( 'NONE', #8420 ) ;
#7674 = DIRECTION ( 'NONE',  ( 0.000000000000000000, -1.000000000000000000, 0.000000000000000000 ) ) ;
#7675 = CARTESIAN_POINT ( 'NONE',  ( 0.2356240016490815659, 0.4776900717921119810, 1.747047244094488194 ) ) ;
#7676 = DIRECTION ( 'NONE',  ( -0.000000000000000000, -0.000000000000000000, 1.000000000000000000 ) ) ;
#7677 = CARTESIAN_POINT ( 'NONE',  ( -1.197070535079588716, 0.07874015748031491790, -1.197070535079588716 ) ) ;
#7678 = ADVANCED_FACE ( 'NONE', ( #8289 ), #21549, .F. ) ;
#7679 = ORIENTED_EDGE ( 'NONE', *, *, #21647, .F. ) ;
#7680 = DIRECTION ( 'NONE',  ( 0.04074159081867598925, 0.000000000000000000, 0.9991697167036057703 ) ) ;
#7681 = CARTESIAN_POINT ( 'NONE',  ( 0.3937007874015748254, 0.9055118110236221041, 0.000000000000000000 ) ) ;
#7682 = CARTESIAN_POINT ( 'NONE',  ( -0.1285103288269285327, -0.3545966721392122545, 0.1992125984251968684 ) ) ;
#7683 = ORIENTED_EDGE ( 'NONE', *, *, #14494, .T. ) ;
#7684 = AXIS2_PLACEMENT_3D ( 'NONE', #17676, #26296, #11325 ) ;
#7685 = DIRECTION ( 'NONE',  ( 0.000000000000000000, 1.000000000000000000, 0.000000000000000000 ) ) ;
#7686 = ORIENTED_EDGE ( 'NONE', *, *, #1886, .T. ) ;
#7687 = CARTESIAN_POINT ( 'NONE',  ( -0.09842519685039370636, 2.800920866141732248E-17, 0.09092130223458683158 ) ) ;
#7688 = AXIS2_PLACEMENT_3D ( 'NONE', #12269, #25125, #16378 ) ;
#7689 = CARTESIAN_POINT ( 'NONE',  ( -0.2490711204941346568, 0.7655264129003995777, -0.7689379837741201484 ) ) ;
#7690 = CARTESIAN_POINT ( 'NONE',  ( 0.1493472610806836354, -0.2230244025072592728, 0.4251224429483507206 ) ) ;
#7691 = DIRECTION ( 'NONE',  ( 1.000000000000000000, 0.000000000000000000, 0.000000000000000000 ) ) ;
#7692 = FACE_OUTER_BOUND ( 'NONE', #14145, .T. ) ;
#7693 = CARTESIAN_POINT ( 'NONE',  ( 0.5890517850735842442, -0.1846255037454771764, 0.07874015748031495954 ) ) ;
#7694 = ORIENTED_EDGE ( 'NONE', *, *, #23278, .T. ) ;
#7695 = CARTESIAN_POINT ( 'NONE',  ( -0.2299571666338338372, 0.2748389101991166039, 0.1805249803347109272 ) ) ;
#7696 = DIRECTION ( 'NONE',  ( -1.000000000000000000, 0.000000000000000000, 0.000000000000000000 ) ) ;
#7697 = EDGE_CURVE ( 'NONE', #10270, #9314, #14969, .T. ) ;
#7698 = AXIS2_PLACEMENT_3D ( 'NONE', #7723, #16336, #1773 ) ;
#7699 = CARTESIAN_POINT ( 'NONE',  ( 1.687505431895960050E-16, 0.3543307086614172485, -1.377952755905512472 ) ) ;
#7700 = CARTESIAN_POINT ( 'NONE',  ( -0.1791085948260308092, -0.3102804211135123946, -3.115157480314960203 ) ) ;
#7701 = EDGE_CURVE ( 'NONE', #23891, #18882, #3182, .T. ) ;
#7702 = UNCERTAINTY_MEASURE_WITH_UNIT (LENGTH_MEASURE( 1.000000000000000082E-05 ), #15259, 'distance_accuracy_value', 'NONE') ;
#7703 = VERTEX_POINT ( 'NONE', #21696 ) ;
#7704 = CARTESIAN_POINT ( 'NONE',  ( -0.3411003281196917092, 0.2991932138496784521, -1.934055118110236338 ) ) ;
#7705 = ADVANCED_FACE ( 'NONE', ( #23552 ), #10669, .F. ) ;
#7706 = CARTESIAN_POINT ( 'NONE',  ( -0.6806799598997224088, 0.05663649493104071925, -0.2380830294301988226 ) ) ;
#7707 = VECTOR ( 'NONE', #15246, 39.37007874015748854 ) ;
#7708 = ORIENTED_EDGE ( 'NONE', *, *, #1280, .T. ) ;
#7709 = ORIENTED_EDGE ( 'NONE', *, *, #19745, .F. ) ;
#7710 = CARTESIAN_POINT ( 'NONE',  ( 0.5781866216489107702, 0.4620966632771911220, 0.2161412452773199544 ) ) ;
#7711 = CARTESIAN_POINT ( 'NONE',  ( 0.000000000000000000, 0.5905511811023621549, -0.3937007874015748254 ) ) ;
#7712 = CARTESIAN_POINT ( 'NONE',  ( -0.3242071728275120468, 0.4225965726692976765, 1.747047244094488194 ) ) ;
#7713 = ORIENTED_EDGE ( 'NONE', *, *, #19012, .F. ) ;
#7714 = ORIENTED_EDGE ( 'NONE', *, *, #17953, .F. ) ;
#7715 = CIRCLE ( 'NONE', #23522, 0.1181010187939084827 ) ;
#7716 = CARTESIAN_POINT ( 'NONE',  ( -0.04928467685644277035, -0.3740848232703729015, -3.100567304031765392 ) ) ;
#7717 = DIRECTION ( 'NONE',  ( 0.8660254037844385966, -0.4999999999999998335, 0.000000000000000000 ) ) ;
#7718 = CARTESIAN_POINT ( 'NONE',  ( -0.3338887748335582772, -5.862181872755905604E-06, -1.869015748010449007 ) ) ;
#7719 = EDGE_LOOP ( 'NONE', ( #19300, #2366 ) ) ;
#7720 = ORIENTED_EDGE ( 'NONE', *, *, #22320, .F. ) ;
#7721 = DIRECTION ( 'NONE',  ( 0.000000000000000000, 0.000000000000000000, 1.000000000000000000 ) ) ;
#7722 = CARTESIAN_POINT ( 'NONE',  ( -0.1599629598573824862, -0.4411872753631803090, 0.07637795275590551769 ) ) ;
#7723 = CARTESIAN_POINT ( 'NONE',  ( -0.3661417322834645272, -0.4724409448818898127, -0.8182917201112815953 ) ) ;
#7724 = CARTESIAN_POINT ( 'NONE',  ( 0.3535065162672724748, -0.2712027394948692827, -1.934055118110236338 ) ) ;
#7725 = ORIENTED_EDGE ( 'NONE', *, *, #27857, .F. ) ;
#7726 = EDGE_LOOP ( 'NONE', ( #12124, #7531, #19942, #14707 ) ) ;
#7727 = DIRECTION ( 'NONE',  ( 0.8660254037844390407, -0.4999999999999994449, 0.000000000000000000 ) ) ;
#7728 = SPHERICAL_SURFACE ( 'NONE', #27559, 0.1299232283464566984 ) ;
#7729 = AXIS2_PLACEMENT_3D ( 'NONE', #19711, #26198, #13469 ) ;
#7730 = FACE_OUTER_BOUND ( 'NONE', #4879, .T. ) ;
#7731 = CARTESIAN_POINT ( 'NONE',  ( 0.3223547283257516272, 0.3832433309296771617, 0.2574803149606298969 ) ) ;
#7732 = CARTESIAN_POINT ( 'NONE',  ( -0.09842519685039370636, 0.07874015748031495954, -0.04546065111729338803 ) ) ;
#7733 = CARTESIAN_POINT ( 'NONE',  ( -0.3988311005573527690, 0.4763376377694653607, 0.2574803149606298969 ) ) ;
#7734 = ( BOUNDED_CURVE ( )  B_SPLINE_CURVE ( 2, ( #880, #24585, #7502 ),
 .UNSPECIFIED., .F., .T. ) 
 B_SPLINE_CURVE_WITH_KNOTS ( ( 3, 3 ),
 ( 0.000000000000000000, 0.1168436138077912356 ),
 .UNSPECIFIED. ) 
 CURVE ( )  GEOMETRIC_REPRESENTATION_ITEM ( )  RATIONAL_B_SPLINE_CURVE ( ( 1.000000000000000000, 1.077350269189625731, 1.077350269189625953 ) ) 
 REPRESENTATION_ITEM ( '' )  ) ;
#7735 = STYLED_ITEM ( 'NONE', ( #24238 ), #21876 ) ;
#7736 = DIRECTION ( 'NONE',  ( 1.000000000000000000, 0.000000000000000000, 0.000000000000000000 ) ) ;
#7737 = CARTESIAN_POINT ( 'NONE',  ( 0.4790450267203003598, 0.08506312950115990645, 0.1075369453498891542 ) ) ;
#7738 = CARTESIAN_POINT ( 'NONE',  ( -0.2395669291338582696, 0.000000000000000000, 0.000000000000000000 ) ) ;
#7739 = EDGE_LOOP ( 'NONE', ( #17604, #13238, #24828, #22597, #22581, #20039, #8418 ) ) ;
#7740 = CARTESIAN_POINT ( 'NONE',  ( -0.5379168165870180651, -0.3108204284649448423, 0.2574827755769819038 ) ) ;
#7741 = CARTESIAN_POINT ( 'NONE',  ( -0.4790450267015415875, 0.08506312949784111677, 0.1075369453641766698 ) ) ;
#7742 = DIRECTION ( 'NONE',  ( -1.000000000000000000, 0.000000000000000000, 0.000000000000000000 ) ) ;
#7743 = ORIENTED_EDGE ( 'NONE', *, *, #16614, .F. ) ;
#7744 = CARTESIAN_POINT ( 'NONE',  ( -0.3268074212154853941, -0.1882834141668338901, 0.07637630750536809898 ) ) ;
#7745 = DIRECTION ( 'NONE',  ( 0.000000000000000000, 1.000000000000000000, 0.000000000000000000 ) ) ;
#7746 = CARTESIAN_POINT ( 'NONE',  ( -0.1712563538833044852, 0.5043504886477827576, 1.747047244094488194 ) ) ;
#7747 = CARTESIAN_POINT ( 'NONE',  ( 0.2268096725222443211, -0.4600326175560562336, 1.766732283464566899 ) ) ;
#7748 = ORIENTED_EDGE ( 'NONE', *, *, #8491, .T. ) ;
#7749 = CONICAL_SURFACE ( 'NONE', #970, 0.1074461786882927178, 1.047197550000000144 ) ;
#7750 = ORIENTED_EDGE ( 'NONE', *, *, #12547, .F. ) ;
#7751 = CARTESIAN_POINT ( 'NONE',  ( -0.1791601451668828893, 0.3102476824511414266, -3.115157480314960647 ) ) ;
#7752 = EDGE_LOOP ( 'NONE', ( #7667, #22292, #1669, #20527, #1859, #13973 ) ) ;
#7753 = CARTESIAN_POINT ( 'NONE',  ( 0.2243259791912049217, -0.6183223858000764794, 0.1461456498277223237 ) ) ;
#7754 = EDGE_CURVE ( 'NONE', #23007, #214, #12794, .T. ) ;
#7755 = DIRECTION ( 'NONE',  ( 0.000000000000000000, -1.000000000000000000, 0.000000000000000000 ) ) ;
#7756 = ORIENTED_EDGE ( 'NONE', *, *, #13522, .F. ) ;
#7757 = EDGE_CURVE ( 'NONE', #23920, #6276, #9061, .T. ) ;
#7758 = ORIENTED_EDGE ( 'NONE', *, *, #8296, .F. ) ;
#7759 = CARTESIAN_POINT ( 'NONE',  ( 0.2466292688015061796, 0.4270824798167727199, -1.569881889763779625 ) ) ;
#7760 = CARTESIAN_POINT ( 'NONE',  ( 0.4339912984563291110, -0.2498791196563492356, 0.09685039370078740717 ) ) ;
#7761 = ORIENTED_EDGE ( 'NONE', *, *, #3879, .T. ) ;
#7762 = ORIENTED_EDGE ( 'NONE', *, *, #17027, .T. ) ;
#7763 = EDGE_CURVE ( 'NONE', #2791, #3990, #5720, .T. ) ;
#7764 = ORIENTED_EDGE ( 'NONE', *, *, #2229, .T. ) ;
#7765 = ITEM_DEFINED_TRANSFORMATION ( 'NONE', 'NONE', #12963,  #11588 ) ;
#7766 = EDGE_CURVE ( 'NONE', #21688, #152, #2194, .T. ) ;
#7767 = CARTESIAN_POINT ( 'NONE',  ( 0.000000000000000000, 0.000000000000000000, -0.1181010187644645215 ) ) ;
#7768 = CARTESIAN_POINT ( 'NONE',  ( 0.4622285577935968948, 0.08111201067590689817, 0.1992142434433712694 ) ) ;
#7769 = CARTESIAN_POINT ( 'NONE',  ( -0.7874015748031496509, 0.9829781505553011334, -0.2190361720152886049 ) ) ;
#7770 = PRODUCT_DEFINITION_SHAPE ( 'NONE', 'NONE',  #1533 ) ;
#7771 = TOROIDAL_SURFACE ( 'NONE', #23573, 0.6102362204724409711, 0.1299212598425196763 ) ;
#7772 = DIRECTION ( 'NONE',  ( 0.000000000000000000, 0.000000000000000000, 1.000000000000000000 ) ) ;
#7773 = ORIENTED_EDGE ( 'NONE', *, *, #9099, .F. ) ;
#7774 = DIRECTION ( 'NONE',  ( 0.000000000000000000, 0.000000000000000000, -1.000000000000000000 ) ) ;
#7775 = DIRECTION ( 'NONE',  ( 0.000000000000000000, -1.000000000000000000, 0.000000000000000000 ) ) ;
#7776 = AXIS2_PLACEMENT_3D ( 'NONE', #24950, #5611, #8565 ) ;
#7777 = DIRECTION ( 'NONE',  ( -0.2036417511401760472, -0.4895227362422912565, 0.8478782506317888989 ) ) ;
#7778 = DIRECTION ( 'NONE',  ( -1.000000000000000000, 0.000000000000000000, 0.000000000000000000 ) ) ;
#7779 = CARTESIAN_POINT ( 'NONE',  ( -0.4921259842519685179, 3.013402556957069934E-17, -1.569881889763779625 ) ) ;
#7780 = FACE_OUTER_BOUND ( 'NONE', #6876, .T. ) ;
#7781 = ORIENTED_EDGE ( 'NONE', *, *, #16423, .T. ) ;
#7782 = CARTESIAN_POINT ( 'NONE',  ( 0.2956505864974370290, 0.3532288989643546095, 0.1639447408648230242 ) ) ;
#7783 = ORIENTED_EDGE ( 'NONE', *, *, #17921, .F. ) ;
#7784 = ORIENTED_EDGE ( 'NONE', *, *, #22572, .F. ) ;
#7785 = VECTOR ( 'NONE', #16974, 39.37007874015748143 ) ;
#7786 = CARTESIAN_POINT ( 'NONE',  ( 0.4035433070866141780, 0.7874015748031496509, 0.000000000000000000 ) ) ;
#7787 = DIMENSIONAL_EXPONENTS ( 1.000000000000000000, 0.000000000000000000, 0.000000000000000000, 0.000000000000000000, 0.000000000000000000, 0.000000000000000000, 0.000000000000000000 ) ;
#7788 = EDGE_LOOP ( 'NONE', ( #1013, #7093, #10922, #23915, #20878, #941 ) ) ;
#7789 = EDGE_CURVE ( 'NONE', #1806, #22055, #90, .T. ) ;
#7790 = DIRECTION ( 'NONE',  ( 0.000000000000000000, 0.000000000000000000, 1.000000000000000000 ) ) ;
#7791 = EDGE_LOOP ( 'NONE', ( #9120, #27812, #8319, #7022 ) ) ;
#7792 = CIRCLE ( 'NONE', #8257, 0.07910393700787400617 ) ;
#7793 = CARTESIAN_POINT ( 'NONE',  ( -0.2255758929756846998, -0.6217623271424783660, 0.1926811207753210409 ) ) ;
#7794 = EDGE_CURVE ( 'NONE', #17730, #7534, #15824, .T. ) ;
#7795 = CARTESIAN_POINT ( 'NONE',  ( 0.1522836969735573143, 0.000000000000000000, 0.000000000000000000 ) ) ;
#7796 = ORIENTED_EDGE ( 'NONE', *, *, #12460, .T. ) ;
#7797 = ADVANCED_FACE ( 'NONE', ( #26066 ), #6218, .F. ) ;
#7798 = ORIENTED_EDGE ( 'NONE', *, *, #15691, .T. ) ;
#7799 = EDGE_LOOP ( 'NONE', ( #5936, #15650 ) ) ;
#7800 = DIRECTION ( 'NONE',  ( 0.000000000000000000, 0.000000000000000000, 1.000000000000000000 ) ) ;
#7801 = CARTESIAN_POINT ( 'NONE',  ( -0.2268096725200377806, -0.4600326175569655618, -1.550196850393700920 ) ) ;
#7802 = CIRCLE ( 'NONE', #10944, 0.1181102362204720091 ) ;
#7803 = EDGE_CURVE ( 'NONE', #23473, #5489, #774, .T. ) ;
#7804 = DIRECTION ( 'NONE',  ( 1.000000000000000000, 0.000000000000000000, 0.000000000000000000 ) ) ;
#7805 = AXIS2_PLACEMENT_3D ( 'NONE', #21105, #23523, #10080 ) ;
#7806 = CARTESIAN_POINT ( 'NONE',  ( -0.5335524835332334792, -0.1429116519061227608, 0.9202755905511811330 ) ) ;
#7807 = CARTESIAN_POINT ( 'NONE',  ( 6.136516277395897527E-17, 0.2165354330708661457, -3.646653543307086576 ) ) ;
#7808 = DIRECTION ( 'NONE',  ( 0.000000000000000000, 1.000000000000000000, 0.000000000000000000 ) ) ;
#7809 = VERTEX_POINT ( 'NONE', #634 ) ;
#7810 = DIRECTION ( 'NONE',  ( 0.000000000000000000, 0.000000000000000000, -1.000000000000000000 ) ) ;
#7811 = AXIS2_PLACEMENT_3D ( 'NONE', #24026, #20060, #4944 ) ;
#7812 = FILL_AREA_STYLE_COLOUR ( '', #24372 ) ;
#7813 = DIRECTION ( 'NONE',  ( 0.000000000000000000, 1.000000000000000000, 0.000000000000000000 ) ) ;
#7814 = CARTESIAN_POINT ( 'NONE',  ( 3.606039370078740678E-16, 0.000000000000000000, 0.000000000000000000 ) ) ;
#7815 = ORIENTED_EDGE ( 'NONE', *, *, #21103, .F. ) ;
#7816 = DIRECTION ( 'NONE',  ( 0.4998319442670609569, 0.000000000000000000, -0.8661224090682619892 ) ) ;
#7817 = CARTESIAN_POINT ( 'NONE',  ( 0.000000000000000000, 0.1968503937007875237, 0.000000000000000000 ) ) ;
#7818 = DIRECTION ( 'NONE',  ( 1.000000000000000000, 0.000000000000000000, 0.000000000000000000 ) ) ;
#7819 = CARTESIAN_POINT ( 'NONE',  ( 0.3976891862754212137, 0.8566358266442657410, -0.5893543329197449276 ) ) ;
#7820 = EDGE_CURVE ( 'NONE', #22680, #24641, #6824, .T. ) ;
#7821 = EDGE_LOOP ( 'NONE', ( #5092, #5307 ) ) ;
#7822 = CIRCLE ( 'NONE', #15061, 0.4807043897637795493 ) ;
#7823 = CARTESIAN_POINT ( 'NONE',  ( -0.0007882571242873708667, 0.7401570605738059250, 0.2562996996008273243 ) ) ;
#7824 = ORIENTED_EDGE ( 'NONE', *, *, #23726, .F. ) ;
#7825 = TOROIDAL_SURFACE ( 'NONE', #23183, 0.3740157480314960647, 0.03937007874015747977 ) ;
#7826 = CARTESIAN_POINT ( 'NONE',  ( 0.2420394123212937232, 0.2892587550802425134, 0.07637795275590551769 ) ) ;
#7827 = LINE ( 'NONE', #22233, #27825 ) ;
#7828 = CONICAL_SURFACE ( 'NONE', #17300, 0.3039508883504944969, 0.2407725888118948110 ) ;
#7829 = CARTESIAN_POINT ( 'NONE',  ( 2.664928230027803213, -0.4724409448818898127, -0.8182917201112815953 ) ) ;
#7830 = LINE ( 'NONE', #20113, #5400 ) ;
#7831 = CARTESIAN_POINT ( 'NONE',  ( -0.5177165354330708347, -0.4724409448818898127, 0.9954570744419881656 ) ) ;
#7832 = ORIENTED_EDGE ( 'NONE', *, *, #709, .T. ) ;
#7833 = FACE_OUTER_BOUND ( 'NONE', #22512, .T. ) ;
#7834 = EDGE_CURVE ( 'NONE', #21486, #25722, #11635, .T. ) ;
#7835 = ORIENTED_EDGE ( 'NONE', *, *, #23596, .F. ) ;
#7836 = CARTESIAN_POINT ( 'NONE',  ( 0.000000000000000000, 0.000000000000000000, -0.1464516454673935042 ) ) ;
#7837 = CARTESIAN_POINT ( 'NONE',  ( -0.4837521785345547665, -0.1097523286755377608, 0.1734435147577276792 ) ) ;
#7838 = AXIS2_PLACEMENT_3D ( 'NONE', #6353, #16809, #25565 ) ;
#7839 = CARTESIAN_POINT ( 'NONE',  ( 0.1512183756281006430, 0.4867863319339526540, 0.04701115990132218730 ) ) ;
#7840 = AXIS2_PLACEMENT_3D ( 'NONE', #1683, #9877, #12426 ) ;
#7841 = CARTESIAN_POINT ( 'NONE',  ( -0.2181214148710382827, -0.2842163005027896761, -3.115157480314960203 ) ) ;
#7842 = CARTESIAN_POINT ( 'NONE',  ( -0.0006443779181934992202, 0.4960456921228240112, 0.1734435147396095056 ) ) ;
#7843 = APPLICATION_CONTEXT ( 'automotive_design' ) ;
#7844 = ORIENTED_EDGE ( 'NONE', *, *, #27521, .T. ) ;
#7845 = CIRCLE ( 'NONE', #8743, 0.3031496062992122820 ) ;
#7846 = CARTESIAN_POINT ( 'NONE',  ( 0.2938049579018460755, 0.3349573549949649842, -1.934055118110236338 ) ) ;
#7847 = ORIENTED_EDGE ( 'NONE', *, *, #27863, .T. ) ;
#7848 = CARTESIAN_POINT ( 'NONE',  ( -0.3376790527244098450, -1.225034693736185121, -0.6364355922310138691 ) ) ;
#7849 = CARTESIAN_POINT ( 'NONE',  ( -0.5043504886477523375, 0.1712563538833050680, 1.747047244094488194 ) ) ;
#7850 = VERTEX_POINT ( 'NONE', #24083 ) ;
#7851 = CARTESIAN_POINT ( 'NONE',  ( -0.1968503937007874127, 0.000000000000000000, 0.09092130223458683158 ) ) ;
#7852 = ORIENTED_EDGE ( 'NONE', *, *, #522, .F. ) ;
#7854 = ADVANCED_FACE ( 'NONE', ( #7257 ), #22602, .F. ) ;
#7853 = CIRCLE ( 'NONE', #24093, 0.8163976377952757435 ) ;
#7855 = CARTESIAN_POINT ( 'NONE',  ( 0.3384212623783103835, 0.1668516812751408562, -3.100567304031765392 ) ) ;
#7856 = AXIS2_PLACEMENT_3D ( 'NONE', #7205, #13697, #22180 ) ;
#7857 = DIRECTION ( 'NONE',  ( 1.000000000000000000, 0.000000000000000000, 0.000000000000000000 ) ) ;
#7858 = CARTESIAN_POINT ( 'NONE',  ( 0.1120675189988346587, -0.5599717622282432972, -0.2558308786799980417 ) ) ;
#7859 = ADVANCED_FACE ( 'NONE', ( #4718 ), #4994, .F. ) ;
#7860 = CARTESIAN_POINT ( 'NONE',  ( 0.01288382760289894825, 0.2165354330708661457, -3.646653543307086576 ) ) ;
#7861 = ORIENTED_EDGE ( 'NONE', *, *, #21916, .T. ) ;
#7862 = CARTESIAN_POINT ( 'NONE',  ( -0.2089723435111590921, -0.4324731448915377641, 0.2362204724409450174 ) ) ;
#7863 = DIRECTION ( 'NONE',  ( 0.6427876096865398070, 0.7660444431189775694, -0.000000000000000000 ) ) ;
#7864 = CARTESIAN_POINT ( 'NONE',  ( -0.5905511811023621549, 0.000000000000000000, 0.000000000000000000 ) ) ;
#7865 = AXIS2_PLACEMENT_3D ( 'NONE', #13421, #17661, #26839 ) ;
#7866 = B_SPLINE_CURVE_WITH_KNOTS ( 'NONE', 3,
 ( #22566, #11543, #11682, #13809, #1243, #22425, #962, #3191, #11824, #8162 ),
 .UNSPECIFIED., .F., .F.,
 ( 4, 2, 2, 2, 4 ),
 ( 0.000000000000000000, 0.2499999999999998890, 0.4999999999999997780, 0.7499999999999996669, 1.000000000000000000 ),
 .UNSPECIFIED. ) ;
#7867 = CARTESIAN_POINT ( 'NONE',  ( -0.09269288654273742656, -0.3460635936745020680, -3.115157480314960647 ) ) ;
#7868 = DIRECTION ( 'NONE',  ( 0.000000000000000000, 0.000000000000000000, -1.000000000000000000 ) ) ;
#7869 = DIRECTION ( 'NONE',  ( 1.000000000000000000, 0.000000000000000000, 0.000000000000000000 ) ) ;
#7870 = DIRECTION ( 'NONE',  ( 0.000000000000000000, 0.000000000000000000, -1.000000000000000000 ) ) ;
#7871 = EDGE_CURVE ( 'NONE', #18812, #10946, #13575, .T. ) ;
#7872 = FACE_OUTER_BOUND ( 'NONE', #27591, .T. ) ;
#7873 = CIRCLE ( 'NONE', #1102, 0.5322834645669292097 ) ;
#7874 = DIRECTION ( 'NONE',  ( -0.000000000000000000, -1.000000000000000000, -0.000000000000000000 ) ) ;
#7875 = CARTESIAN_POINT ( 'NONE',  ( 0.4688657571939683910, 0.08326155277437964630, 0.1212655228563162269 ) ) ;
#7876 = AXIS2_PLACEMENT_3D ( 'NONE', #8330, #25560, #6217 ) ;
#7877 = CARTESIAN_POINT ( 'NONE',  ( -0.2965233727166468047, 0.3524965443697193335, 0.1771653543307085965 ) ) ;
#7878 = ORIENTED_EDGE ( 'NONE', *, *, #23993, .T. ) ;
#7879 = CARTESIAN_POINT ( 'NONE',  ( -0.5672097974520583508, 0.07461436618597647175, 0.9399606299212600602 ) ) ;
#7880 = CARTESIAN_POINT ( 'NONE',  ( -0.3713448905834433322, 0.06600512665679449109, 0.1992125984251968684 ) ) ;
#7881 = B_SPLINE_CURVE_WITH_KNOTS ( 'NONE', 3,
 ( #17517, #4251, #8483, #1984, #12856, #26135 ),
 .UNSPECIFIED., .F., .F.,
 ( 4, 2, 4 ),
 ( -1.199999999999999956, -0.5999999999999999778, 0.000000000000000000 ),
 .UNSPECIFIED. ) ;
#7882 = ORIENTED_EDGE ( 'NONE', *, *, #12632, .F. ) ;
#7883 = CARTESIAN_POINT ( 'NONE',  ( 0.000000000000000000, 0.09092130223458683158, -0.4724409448818898127 ) ) ;
#7884 = DIRECTION ( 'NONE',  ( 0.000000000000000000, 0.000000000000000000, 1.000000000000000000 ) ) ;
#7885 = CARTESIAN_POINT ( 'NONE',  ( 0.04956879728060044343, 0.2165354330708660624, -3.634230943735654140 ) ) ;
#7886 = TOROIDAL_SURFACE ( 'NONE', #20941, 0.5610236220472440971, 0.1003937007874015908 ) ;
#7887 = ORIENTED_EDGE ( 'NONE', *, *, #267, .T. ) ;
#7888 = VERTEX_POINT ( 'NONE', #2862 ) ;
#7889 = CARTESIAN_POINT ( 'NONE',  ( 0.1259842519685039353, -0.1751968503937007815, -2.466516690495447540E-17 ) ) ;
#7890 = ORIENTED_EDGE ( 'NONE', *, *, #23474, .T. ) ;
#7891 = EDGE_CURVE ( 'NONE', #9309, #17480, #14035, .T. ) ;
#7892 = CARTESIAN_POINT ( 'NONE',  ( 0.2161007281681049663, -0.5956855348339761269, 0.2481708550939305813 ) ) ;
#7893 = ADVANCED_FACE ( 'NONE', ( #26334 ), #6995, .F. ) ;
#7894 = DIRECTION ( 'NONE',  ( 1.000000000000000000, 0.000000000000000000, 0.000000000000000000 ) ) ;
#7895 = ORIENTED_EDGE ( 'NONE', *, *, #17101, .T. ) ;
#7896 = ORIENTED_EDGE ( 'NONE', *, *, #25971, .F. ) ;
#7897 = AXIS2_PLACEMENT_3D ( 'NONE', #4239, #10442, #8342 ) ;
#7898 = CARTESIAN_POINT ( 'NONE',  ( 0.4423390553432353656, -0.2180862235769564228, -1.550196850393700920 ) ) ;
#7899 = AXIS2_PLACEMENT_3D ( 'NONE', #8221, #24734, #25160 ) ;
#7900 = ORIENTED_EDGE ( 'NONE', *, *, #3968, .F. ) ;
#7901 = CYLINDRICAL_SURFACE ( 'NONE', #6839, 0.1181102362204718703 ) ;
#7902 = ORIENTED_EDGE ( 'NONE', *, *, #21479, .F. ) ;
#7903 = ITEM_DEFINED_TRANSFORMATION ( 'NONE', 'NONE', #22398,  #11588 ) ;
#7904 = DIRECTION ( 'NONE',  ( -0.000000000000000000, -1.000000000000000000, -0.000000000000000000 ) ) ;
#7905 = B_SPLINE_CURVE_WITH_KNOTS ( 'NONE', 3,
 ( #832, #7892, #9561, #973, #24829, #1253, #7753, #14260, #22290, #16366 ),
 .UNSPECIFIED., .F., .F.,
 ( 4, 2, 2, 2, 4 ),
 ( 0.000000000000000000, 0.2500000000000003331, 0.5000000000000002220, 0.7500000000000001110, 1.000000000000000000 ),
 .UNSPECIFIED. ) ;
#7906 = FACE_OUTER_BOUND ( 'NONE', #2524, .T. ) ;
#7907 = DIRECTION ( 'NONE',  ( 0.000000000000000000, 0.000000000000000000, -1.000000000000000000 ) ) ;
#7908 = AXIS2_PLACEMENT_3D ( 'NONE', #27376, #20735, #27234 ) ;
#7909 = ORIENTED_EDGE ( 'NONE', *, *, #23726, .T. ) ;
#7910 = CARTESIAN_POINT ( 'NONE',  ( 0.000000000000000000, 0.000000000000000000, 0.01181102362204724393 ) ) ;
#7911 = UNCERTAINTY_MEASURE_WITH_UNIT (LENGTH_MEASURE( 1.000000000000000082E-05 ), #15768, 'distance_accuracy_value', 'NONE') ;
#7912 = CARTESIAN_POINT ( 'NONE',  ( 3.168943700787402105E-16, -1.183070866141732402, 6.774128948039492984E-17 ) ) ;
#7913 = EDGE_CURVE ( 'NONE', #3462, #21723, #18046, .T. ) ;
#7914 = CARTESIAN_POINT ( 'NONE',  ( 0.000000000000000000, 0.3937007873309092409, -2.066929133858267598 ) ) ;
#7915 = DIRECTION ( 'NONE',  ( 0.000000000000000000, 0.000000000000000000, 1.000000000000000000 ) ) ;
#7916 = CARTESIAN_POINT ( 'NONE',  ( -0.5385832331986013521, -0.4187149276795443242, 0.1663235595950885437 ) ) ;
#7917 = AXIS2_PLACEMENT_3D ( 'NONE', #9035, #15818, #15286 ) ;
#7918 = CARTESIAN_POINT ( 'NONE',  ( 0.000000000000000000, -0.1136516277932334562, 0.1968503937007874127 ) ) ;
#7919 = CARTESIAN_POINT ( 'NONE',  ( 0.000000000000000000, -0.1751968503937007815, 2.466516690495447540E-17 ) ) ;
#7920 = ORIENTED_EDGE ( 'NONE', *, *, #18017, .F. ) ;
#7921 = EDGE_CURVE ( 'NONE', #3844, #11261, #21266, .T. ) ;
#7922 = ORIENTED_EDGE ( 'NONE', *, *, #20571, .F. ) ;
#7923 = DIRECTION ( 'NONE',  ( 1.000000000000000000, 0.000000000000000000, 0.000000000000000000 ) ) ;
#7924 = CARTESIAN_POINT ( 'NONE',  ( 0.1291602287245497971, -0.3543605079199910191, 0.07637549214372835182 ) ) ;
#7925 = AXIS2_PLACEMENT_3D ( 'NONE', #7239, #898, #3266 ) ;
#7926 = ORIENTED_EDGE ( 'NONE', *, *, #15699, .T. ) ;
#7927 = CARTESIAN_POINT ( 'NONE',  ( 0.3012109481301854519, 0.3598698725862389813, 0.1992125984251968684 ) ) ;
#7928 = FACE_OUTER_BOUND ( 'NONE', #14771, .T. ) ;
#7929 = CARTESIAN_POINT ( 'NONE',  ( 0.4842519685039370358, 5.930376232091513698E-17, -0.01377952755905511792 ) ) ;
#7930 = EDGE_LOOP ( 'NONE', ( #7325, #19866, #12446, #10698, #12578, #11251, #20816, #24832, #10076, #19881, #7900 ) ) ;
#7931 = FACE_BOUND ( 'NONE', #18262, .T. ) ;
#7932 = VERTEX_POINT ( 'NONE', #11091 ) ;
#7933 = DIRECTION ( 'NONE',  ( -1.000000000000000000, 0.000000000000000000, 0.000000000000000000 ) ) ;
#7934 = AXIS2_PLACEMENT_3D ( 'NONE', #21928, #17544, #2553 ) ;
#7935 = CARTESIAN_POINT ( 'NONE',  ( 0.4932821129636645874, 0.08637579872942321990, 0.2574803149606298969 ) ) ;
#7936 = CARTESIAN_POINT ( 'NONE',  ( -0.2239856983880364194, -0.4635973202232746559, 0.3251195115423166637 ) ) ;
#7937 = EDGE_CURVE ( 'NONE', #15244, #14040, #16294, .T. ) ;
#7938 = FACE_OUTER_BOUND ( 'NONE', #7290, .T. ) ;
#7939 = ORIENTED_EDGE ( 'NONE', *, *, #1071, .F. ) ;
#7940 = DIRECTION ( 'NONE',  ( 1.000000000000000000, 0.000000000000000000, 0.000000000000000000 ) ) ;
#7941 = VERTEX_POINT ( 'NONE', #6856 ) ;
#7942 = CARTESIAN_POINT ( 'NONE',  ( 0.2904160862623596517, -0.1677079028045486975, 1.973425196850393970 ) ) ;
#7943 = DIRECTION ( 'NONE',  ( 0.000000000000000000, 1.000000000000000000, 0.000000000000000000 ) ) ;
#7944 = TOROIDAL_SURFACE ( 'NONE', #3869, 0.3872945158171015589, 0.01377952755905511792 ) ;
#7945 = CARTESIAN_POINT ( 'NONE',  ( 0.000000000000000000, 0.000000000000000000, 0.1377952755905511861 ) ) ;
#7946 = CARTESIAN_POINT ( 'NONE',  ( -0.03607471876262562799, -0.5511811023622048555, 0.9399606299212598381 ) ) ;
#7947 = EDGE_CURVE ( 'NONE', #9216, #15905, #7649, .T. ) ;
#7948 = CYLINDRICAL_SURFACE ( 'NONE', #3055, 0.4921259842519685179 ) ;
#7949 = EDGE_CURVE ( 'NONE', #23447, #21391, #19897, .T. ) ;
#7950 = DIRECTION ( 'NONE',  ( -0.000000000000000000, -1.000000000000000000, -0.000000000000000000 ) ) ;
#7951 = EDGE_LOOP ( 'NONE', ( #1824, #14345 ) ) ;
#7952 = CARTESIAN_POINT ( 'NONE',  ( -0.4165721057576322606, 0.3313508221749649763, 0.3401574803149606252 ) ) ;
#7953 = ADVANCED_FACE ( 'NONE', ( #3717 ), #20838, .T. ) ;
#7954 = EDGE_CURVE ( 'NONE', #27013, #14499, #3562, .T. ) ;
#7955 = VECTOR ( 'NONE', #3495, 39.37007874015748143 ) ;
#7956 = CARTESIAN_POINT ( 'NONE',  ( 0.2089723435111816296, -0.4324731448915269394, 0.2194422276813851325 ) ) ;
#7957 = VERTEX_POINT ( 'NONE', #5431 ) ;
#7958 = AXIS2_PLACEMENT_3D ( 'NONE', #21654, #8783, #343 ) ;
#7959 = CARTESIAN_POINT ( 'NONE',  ( 1.798137748274881931, -2.684055118110236116, 0.4406760877627165507 ) ) ;
#7960 = DIRECTION ( 'NONE',  ( 0.000000000000000000, 1.000000000000000000, 0.000000000000000000 ) ) ;
#7961 = CARTESIAN_POINT ( 'NONE',  ( 0.4771018889076559244, 0.3804760601893846794, 0.2362204724409449064 ) ) ;
#7962 = DIRECTION ( 'NONE',  ( 0.000000000000000000, 0.000000000000000000, 1.000000000000000000 ) ) ;
#7963 = VERTEX_POINT ( 'NONE', #27321 ) ;
#7964 = DIRECTION ( 'NONE',  ( 0.000000000000000000, 0.000000000000000000, 1.000000000000000000 ) ) ;
#7965 = ORIENTED_EDGE ( 'NONE', *, *, #16918, .T. ) ;
#7966 = PLANE ( 'NONE',  #20267 ) ;
#7967 = CARTESIAN_POINT ( 'NONE',  ( 0.1136811023622047168, 0.000000000000000000, 0.000000000000000000 ) ) ;
#7968 = CARTESIAN_POINT ( 'NONE',  ( 0.000000000000000000, 0.5511811023622047445, 0.1377952755905511861 ) ) ;
#7969 = DIRECTION ( 'NONE',  ( 0.000000000000000000, 1.000000000000000000, 0.000000000000000000 ) ) ;
#7970 = ORIENTED_EDGE ( 'NONE', *, *, #2043, .F. ) ;
#7971 = CARTESIAN_POINT ( 'NONE',  ( 1.877524803149606209E-16, 0.000000000000000000, 0.4330708661417322913 ) ) ;
#7972 = EDGE_LOOP ( 'NONE', ( #26711, #3602, #23155, #23238 ) ) ;
#7973 = CARTESIAN_POINT ( 'NONE',  ( 0.2979095355689177493, -0.6203660015065670663, 0.3401574803149606252 ) ) ;
#7974 = CYLINDRICAL_SURFACE ( 'NONE', #16940, 0.8163976377952756325 ) ;
#7975 = CARTESIAN_POINT ( 'NONE',  ( 0.1516263115863346334, -0.2937912646890007973, -0.3972688187320929099 ) ) ;
#7976 = CARTESIAN_POINT ( 'NONE',  ( 0.000000000000000000, 0.000000000000000000, -0.05856299212598425896 ) ) ;
#7977 = TOROIDAL_SURFACE ( 'NONE', #23775, 0.5610236220472440971, 0.1003937007874015908 ) ;
#7978 = FACE_OUTER_BOUND ( 'NONE', #15581, .T. ) ;
#7979 = DIMENSIONAL_EXPONENTS ( 1.000000000000000000, 0.000000000000000000, 0.000000000000000000, 0.000000000000000000, 0.000000000000000000, 0.000000000000000000, 0.000000000000000000 ) ;
#7980 = VERTEX_POINT ( 'NONE', #26891 ) ;
#7981 = CARTESIAN_POINT ( 'NONE',  ( 0.3858397471888846408, -0.2228126397719881469, -1.934055118110236338 ) ) ;
#7982 = EDGE_CURVE ( 'NONE', #6078, #2920, #25303, .T. ) ;
#7983 = EDGE_CURVE ( 'NONE', #9494, #9714, #22658, .T. ) ;
#7984 = ORIENTED_EDGE ( 'NONE', *, *, #7491, .F. ) ;
#7985 = ORIENTED_EDGE ( 'NONE', *, *, #20054, .F. ) ;
#7986 = ORIENTED_EDGE ( 'NONE', *, *, #20028, .F. ) ;
#7987 = ORIENTED_EDGE ( 'NONE', *, *, #12632, .T. ) ;
#7988 = CARTESIAN_POINT ( 'NONE',  ( -0.5172021183779732523, -0.4971257496141905929, 0.1366764242586682998 ) ) ;
#7989 = DIRECTION ( 'NONE',  ( -1.000000000000000000, 0.000000000000000000, 0.000000000000000000 ) ) ;
#7990 = PRODUCT_CONTEXT ( 'NONE', #2576, 'mechanical' ) ;
#7991 = CARTESIAN_POINT ( 'NONE',  ( 0.2564944395515637576, -0.4441657790108029524, 1.747047244094488194 ) ) ;
#7992 = ( NAMED_UNIT ( * ) PLANE_ANGLE_UNIT ( ) SI_UNIT ( $, .RADIAN. ) ) ;
#7993 = EDGE_LOOP ( 'NONE', ( #27242, #1265, #14498, #9901, #17346, #8002 ) ) ;
#7994 = CARTESIAN_POINT ( 'NONE',  ( -0.4539000224940974992, -0.3482225189666513510, 0.9399606299212598381 ) ) ;
#7995 = FACE_OUTER_BOUND ( 'NONE', #18966, .T. ) ;
#7996 = VECTOR ( 'NONE', #18052, 39.37007874015748143 ) ;
#7997 = CARTESIAN_POINT ( 'NONE',  ( 0.3012109481301854519, 0.3598698725862389813, 0.1992125984251968684 ) ) ;
#7998 = PRODUCT_DEFINITION_SHAPE ( 'NONE', 'NONE',  #1882 ) ;
#7999 = CARTESIAN_POINT ( 'NONE',  ( -0.2070393714800602414, -0.07144576004975727868, -0.2362204724409449064 ) ) ;
#8000 = CARTESIAN_POINT ( 'NONE',  ( -0.3362336590883612808, 0.1141709026133623794, 1.953740157480315043 ) ) ;
#8001 = EDGE_CURVE ( 'NONE', #13350, #657, #12194, .T. ) ;
#8002 = ORIENTED_EDGE ( 'NONE', *, *, #16984, .F. ) ;
#8003 = VECTOR ( 'NONE', #3587, 39.37007874015748854 ) ;
#8004 = CARTESIAN_POINT ( 'NONE',  ( -0.5638480983043335781, -0.2075177900316160229, -0.2630347114838766931 ) ) ;
#8006 = CARTESIAN_POINT ( 'NONE',  ( -0.3482225189666627863, 0.4539000224941008854, 0.9399606299212598381 ) ) ;
#8005 = CARTESIAN_POINT ( 'NONE',  ( -0.3289909311256231650, -0.1896185148830505374, -3.100567304031763616 ) ) ;
#8007 = ( REPRESENTATION_RELATIONSHIP ('NONE','NONE', #12434, #16232 ) REPRESENTATION_RELATIONSHIP_WITH_TRANSFORMATION ( #8326 )SHAPE_REPRESENTATION_RELATIONSHIP( ) ) ;
#8008 = EDGE_LOOP ( 'NONE', ( #5661, #14370 ) ) ;
#8009 = CARTESIAN_POINT ( 'NONE',  ( -1.197070535079588716, 0.4724409448818898127, -1.197070535079588716 ) ) ;
#8010 = CARTESIAN_POINT ( 'NONE',  ( 0.4167985568850881561, 0.07349283109919291235, 0.1377952755905511861 ) ) ;
#8011 = CARTESIAN_POINT ( 'NONE',  ( -0.02339816079119098197, 0.3574975638436101444, -3.115157480314960647 ) ) ;
#8012 = CARTESIAN_POINT ( 'NONE',  ( 0.03532354024591720376, -1.576771653543307172, 9.184850993605150903E-17 ) ) ;
#8013 = SPHERICAL_SURFACE ( 'NONE', #9328, 0.1003956692913385851 ) ;
#8014 = CYLINDRICAL_SURFACE ( 'NONE', #670, 0.1308464566929133932 ) ;
#8015 = CARTESIAN_POINT ( 'NONE',  ( -0.3334645669291338987, 0.8103892183150610551, -0.9220603341868013336 ) ) ;
#8016 = CARTESIAN_POINT ( 'NONE',  ( 0.3012109481302311376, 0.3598698725862007897, 0.07637795275590551769 ) ) ;
#8017 = DIRECTION ( 'NONE',  ( -0.000000000000000000, -0.000000000000000000, 1.000000000000000000 ) ) ;
#8018 = ADVANCED_FACE ( 'NONE', ( #10206 ), #7749, .F. ) ;
#8019 = AXIS2_PLACEMENT_3D ( 'NONE', #22783, #23076, #3409 ) ;
#8020 = DIRECTION ( 'NONE',  ( 0.000000000000000000, 0.000000000000000000, 1.000000000000000000 ) ) ;
#8021 = AXIS2_PLACEMENT_3D ( 'NONE', #2469, #21286, #13076 ) ;
#8022 = ADVANCED_FACE ( 'NONE', ( #14334, #7833 ), #12063, .T. ) ;
#8023 = VERTEX_POINT ( 'NONE', #9799 ) ;
#8024 = CYLINDRICAL_SURFACE ( 'NONE', #27341, 0.6889763779527560139 ) ;
#8025 = CARTESIAN_POINT ( 'NONE',  ( -0.03746919241557482988, 0.5708675606921427281, 0.9399606299212600602 ) ) ;
#8026 = DIRECTION ( 'NONE',  ( 0.000000000000000000, 0.000000000000000000, -1.000000000000000000 ) ) ;
#8027 = CARTESIAN_POINT ( 'NONE',  ( 0.5118110236220472231, 3.133938659235352953E-17, 1.766732283464566899 ) ) ;
#8028 = AXIS2_PLACEMENT_3D ( 'NONE', #13458, #5116, #9209 ) ;
#8029 = CARTESIAN_POINT ( 'NONE',  ( 0.000000000000000000, 0.000000000000000000, 0.9399606299212598381 ) ) ;
#8030 = DIRECTION ( 'NONE',  ( 0.000000000000000000, 0.000000000000000000, -1.000000000000000000 ) ) ;
#8031 = CARTESIAN_POINT ( 'NONE',  ( 0.5610236220472440971, 0.000000000000000000, 0.1771653543307086520 ) ) ;
#8032 = CARTESIAN_POINT ( 'NONE',  ( -0.06957181182499248828, -0.5280699926562971713, 1.747047244094488194 ) ) ;
#8033 = CARTESIAN_POINT ( 'NONE',  ( -0.5118110236220472231, -0.03349795313264326835, 1.766732283464566899 ) ) ;
#8034 = ORIENTED_EDGE ( 'NONE', *, *, #26906, .T. ) ;
#8035 = ORIENTED_EDGE ( 'NONE', *, *, #751, .F. ) ;
#8036 = CARTESIAN_POINT ( 'NONE',  ( -0.3102476824511312681, 0.1791601451669032896, -3.115157480314960647 ) ) ;
#8037 = ORIENTED_EDGE ( 'NONE', *, *, #3659, .T. ) ;
#8038 = CARTESIAN_POINT ( 'NONE',  ( -0.4465874321618644172, -0.1200170377978878600, -1.928289503579156960 ) ) ;
#8039 = DIRECTION ( 'NONE',  ( 0.000000000000000000, 1.000000000000000000, 0.000000000000000000 ) ) ;
#8040 = B_SPLINE_CURVE_WITH_KNOTS ( 'NONE', 3,
 ( #17615, #2354, #21997, #10986, #4613, #21862 ),
 .UNSPECIFIED., .F., .F.,
 ( 4, 2, 4 ),
 ( 0.6902184472752670441, 0.6915327610580710438, 0.6928470748408740443 ),
 .UNSPECIFIED. ) ;
#8041 = CARTESIAN_POINT ( 'NONE',  ( -0.2521176338356575508, 0.2211428102655751127, 1.973425196850393970 ) ) ;
#8042 = EDGE_CURVE ( 'NONE', #5560, #20533, #14985, .T. ) ;
#8043 = ORIENTED_EDGE ( 'NONE', *, *, #4386, .F. ) ;
#8044 = CARTESIAN_POINT ( 'NONE',  ( -0.06441834428466408635, -0.4889536969035170877, -1.550196850393700920 ) ) ;
#8045 = DIRECTION ( 'NONE',  ( -0.9749279121818236193, -0.2225209339563142819, 0.000000000000000000 ) ) ;
#8046 = ORIENTED_EDGE ( 'NONE', *, *, #1431, .T. ) ;
#8047 = VERTEX_POINT ( 'NONE', #20678 ) ;
#8048 = EDGE_LOOP ( 'NONE', ( #26457, #8589, #22907, #24505, #23074 ) ) ;
#8049 = MECHANICAL_DESIGN_GEOMETRIC_PRESENTATION_REPRESENTATION (  '', ( #15273 ), #4433 ) ;
#8050 = CARTESIAN_POINT ( 'NONE',  ( -0.3607825703597850042, 0.06309631803674747852, 0.1910323753036148042 ) ) ;
#8051 = CARTESIAN_POINT ( 'NONE',  ( 0.2647715730835492609, -0.5498038367121063086, 0.2362204724409449064 ) ) ;
#8052 = CARTESIAN_POINT ( 'NONE',  ( 0.0005939837304750000086, 0.5007870493127504208, 0.09685039370078740717 ) ) ;
#8053 = CARTESIAN_POINT ( 'NONE',  ( 0.4685039370078740717, 5.737518468446261360E-17, -0.01377952755905511792 ) ) ;
#8054 = ORIENTED_EDGE ( 'NONE', *, *, #8607, .F. ) ;
#8055 = CARTESIAN_POINT ( 'NONE',  ( -0.5905511811023621549, -0.4526313213353574949, 0.9943460912301771426 ) ) ;
#8056 = ADVANCED_FACE ( 'NONE', ( #22520, #3147 ), #3421, .T. ) ;
#8057 = AXIS2_PLACEMENT_3D ( 'NONE', #6660, #4532, #19650 ) ;
#8058 = DIRECTION ( 'NONE',  ( 0.000000000000000000, 0.000000000000000000, -1.000000000000000000 ) ) ;
#8059 = CARTESIAN_POINT ( 'NONE',  ( -2.272295064268543552, 0.6488494047548032384, 2.027559055118110187 ) ) ;
#8060 = EDGE_CURVE ( 'NONE', #21315, #14586, #27045, .T. ) ;
#8061 = CARTESIAN_POINT ( 'NONE',  ( -0.6035792859986336412, -0.1877841116824367773, 0.2224687983481839493 ) ) ;
#8062 = AXIS2_PLACEMENT_3D ( 'NONE', #2270, #13144, #21359 ) ;
#8063 = FACE_OUTER_BOUND ( 'NONE', #6473, .T. ) ;
#8064 = CIRCLE ( 'NONE', #2121, 0.6212598425196850238 ) ;
#8065 = CARTESIAN_POINT ( 'NONE',  ( 0.2428345617565153547, 0.2885915454824177218, 0.1992125984251968684 ) ) ;
#8066 = DIRECTION ( 'NONE',  ( 0.000000000000000000, 0.000000000000000000, -1.000000000000000000 ) ) ;
#8067 = ORIENTED_EDGE ( 'NONE', *, *, #23140, .T. ) ;
#8068 = CIRCLE ( 'NONE', #3988, 0.4010740433761567081 ) ;
#8069 = VERTEX_POINT ( 'NONE', #24910 ) ;
#8070 = VERTEX_POINT ( 'NONE', #5570 ) ;
#8071 = DIRECTION ( 'NONE',  ( 1.000000000000000000, 0.000000000000000000, 0.000000000000000000 ) ) ;
#8072 = CARTESIAN_POINT ( 'NONE',  ( 0.4173228346456693272, 0.000000000000000000, -5.463696850393700654E-18 ) ) ;
#8073 = ORIENTED_EDGE ( 'NONE', *, *, #27737, .T. ) ;
#8074 = CARTESIAN_POINT ( 'NONE',  ( -0.2981382804007346454, -0.6202561546315846774, 0.3401591245381551110 ) ) ;
#8075 = ORIENTED_EDGE ( 'NONE', *, *, #17839, .F. ) ;
#8076 = ADVANCED_FACE ( 'NONE', ( #14198 ), #9512, .F. ) ;
#8077 = CARTESIAN_POINT ( 'NONE',  ( 0.000000000000000000, 0.03937007874015751446, 0.000000000000000000 ) ) ;
#8078 = AXIS2_PLACEMENT_3D ( 'NONE', #16218, #1110, #5479 ) ;
#8079 = TOROIDAL_SURFACE ( 'NONE', #2651, 0.5610236220472440971, 0.1003937007874015908 ) ;
#8080 = CARTESIAN_POINT ( 'NONE',  ( -0.03532354024591893848, -0.8267716535433071723, -0.7500000000000001110 ) ) ;
#8081 = CARTESIAN_POINT ( 'NONE',  ( 0.4895462770358314786, 0.6565912641725563104, -0.5754374930411751965 ) ) ;
#8082 = ORIENTED_EDGE ( 'NONE', *, *, #27125, .F. ) ;
#8083 = CARTESIAN_POINT ( 'NONE',  ( -0.1623262587461356543, -0.4476804331100887602, 0.1212655228106225697 ) ) ;
#8084 = CARTESIAN_POINT ( 'NONE',  ( 0.03532354024591712049, -0.8267716535433071723, 0.000000000000000000 ) ) ;
#8085 = CARTESIAN_POINT ( 'NONE',  ( 0.5085315017394973491, -0.06690352886883006722, -1.550196850393700476 ) ) ;
#8086 = AXIS2_PLACEMENT_3D ( 'NONE', #25581, #8757, #4111 ) ;
#8087 = CARTESIAN_POINT ( 'NONE',  ( 0.08676778863011423704, 0.3239425792934499948, 1.953740157480315043 ) ) ;
#8088 = CARTESIAN_POINT ( 'NONE',  ( 0.5118110236220473341, -0.03349795313024152288, -1.550196850393700920 ) ) ;
#8089 = FACE_OUTER_BOUND ( 'NONE', #1848, .T. ) ;
#8090 = CARTESIAN_POINT ( 'NONE',  ( 0.03607471876262387245, -0.5511811023622048555, 0.9399606299212598381 ) ) ;
#8091 = DIRECTION ( 'NONE',  ( 1.000000000000000000, 0.000000000000000000, 0.000000000000000000 ) ) ;
#8092 = EDGE_LOOP ( 'NONE', ( #10502, #13646, #17576, #1076, #16394, #6174, #7026, #14818 ) ) ;
#8093 = DIRECTION ( 'NONE',  ( 0.000000000000000000, -1.000000000000000000, 0.000000000000000000 ) ) ;
#8094 = CIRCLE ( 'NONE', #9874, 0.8267716535433071723 ) ;
#8095 = ORIENTED_EDGE ( 'NONE', *, *, #19515, .T. ) ;
#8096 = AXIS2_PLACEMENT_3D ( 'NONE', #18577, #7870, #22992 ) ;
#8097 = CIRCLE ( 'NONE', #11186, 0.2395669291338582696 ) ;
#8098 = VERTEX_POINT ( 'NONE', #27751 ) ;
#8099 = CARTESIAN_POINT ( 'NONE',  ( -0.4069448477569480582, 0.3121994997578198539, -1.550196850393700920 ) ) ;
#8100 = DIRECTION ( 'NONE',  ( 0.9887279461703429861, 0.000000000000000000, 0.1497232395514318803 ) ) ;
#8102 = CARTESIAN_POINT ( 'NONE',  ( 0.000000000000000000, 0.09092130223458683158, -0.4724409448818898127 ) ) ;
#8101 = COLOUR_RGB ( '', 0.08235294, 0.09019608, 0.10196078) ;
#8103 = DIRECTION ( 'NONE',  ( 0.000000000000000000, 0.9999999999742198442, -7.180547322999998243E-06 ) ) ;
#8104 = ORIENTED_EDGE ( 'NONE', *, *, #9352, .T. ) ;
#8105 = DIRECTION ( 'NONE',  ( 1.000000000000000000, 0.000000000000000000, 0.000000000000000000 ) ) ;
#8106 = EDGE_LOOP ( 'NONE', ( #23699, #4496, #15215, #3011 ) ) ;
#8107 = DIRECTION ( 'NONE',  ( 0.2036417511401769909, -0.4895227362422910344, 0.8478782506317890100 ) ) ;
#8108 = DIRECTION ( 'NONE',  ( 0.000000000000000000, 0.000000000000000000, 1.000000000000000000 ) ) ;
#8109 = CARTESIAN_POINT ( 'NONE',  ( -0.5905511811023621549, -0.4724409448818898127, 0.8182917201112815953 ) ) ;
#8110 = DIRECTION ( 'NONE',  ( 1.000000000000000000, 0.000000000000000000, 0.000000000000000000 ) ) ;
#8111 = EDGE_CURVE ( 'NONE', #720, #24074, #19460, .T. ) ;
#8112 = EDGE_LOOP ( 'NONE', ( #20430, #3640, #7264, #7852 ) ) ;
#8113 = ( NAMED_UNIT ( * ) PLANE_ANGLE_UNIT ( ) SI_UNIT ( $, .RADIAN. ) ) ;
#8114 = AXIS2_PLACEMENT_3D ( 'NONE', #128, #6315, #8698 ) ;
#8115 = CARTESIAN_POINT ( 'NONE',  ( -0.03532354024591771724, -0.6299212598425196763, 0.000000000000000000 ) ) ;
#8116 = EDGE_CURVE ( 'NONE', #1085, #14294, #23818, .T. ) ;
#8117 = CARTESIAN_POINT ( 'NONE',  ( -0.2361997806693948987, -0.2693761163849906493, -3.115157480314960647 ) ) ;
#8118 = VECTOR ( 'NONE', #7048, 39.37007874015748854 ) ;
#8119 = CARTESIAN_POINT ( 'NONE',  ( 0.2180862235769348290, -0.4423390553432507977, -1.569881889763779625 ) ) ;
#8120 = ORIENTED_EDGE ( 'NONE', *, *, #27089, .T. ) ;
#8121 = CARTESIAN_POINT ( 'NONE',  ( -0.2761764805255463306, -0.3599896729929341621, -1.934055118110236338 ) ) ;
#8122 = CARTESIAN_POINT ( 'NONE',  ( -0.4585215200179055817, 0.03001016326912889221, -1.928289503579156516 ) ) ;
#8123 = ORIENTED_EDGE ( 'NONE', *, *, #15837, .T. ) ;
#8124 = VERTEX_POINT ( 'NONE', #4656 ) ;
#8125 = CARTESIAN_POINT ( 'NONE',  ( -0.5743180011325290657, -0.2548351232479605932, 0.04982753927068897526 ) ) ;
#8126 = CARTESIAN_POINT ( 'NONE',  ( 0.3765118517642104257, -2.263258471485603576E-17, -3.100567304031763172 ) ) ;
#8127 = CARTESIAN_POINT ( 'NONE',  ( -0.5314960629921260393, 0.03478633594543736884, 1.747047244094488194 ) ) ;
#8128 = DIRECTION ( 'NONE',  ( 0.000000000000000000, 1.000000000000000000, 0.000000000000000000 ) ) ;
#8129 = AXIS2_PLACEMENT_3D ( 'NONE', #20253, #3284, #27044 ) ;
#8130 = ORIENTED_EDGE ( 'NONE', *, *, #24794, .T. ) ;
#8131 = EDGE_CURVE ( 'NONE', #21888, #26797, #16759, .T. ) ;
#8132 = CIRCLE ( 'NONE', #1817, 0.6751968503937006982 ) ;
#8133 = LINE ( 'NONE', #21122, #17835 ) ;
#8134 = CARTESIAN_POINT ( 'NONE',  ( -0.1775220790476026711, -0.3075317527318737199, 1.953740157480315043 ) ) ;
#8135 = FACE_BOUND ( 'NONE', #4953, .T. ) ;
#8136 = CARTESIAN_POINT ( 'NONE',  ( 0.000000000000000000, 0.000000000000000000, -0.1033464566929133965 ) ) ;
#8137 = B_SPLINE_CURVE_WITH_KNOTS ( 'NONE', 3,
 ( #22007, #162, #22273, #24125 ),
 .UNSPECIFIED., .F., .F.,
 ( 4, 4 ),
 ( 0.000000000000000000, 1.000000000000000000 ),
 .UNSPECIFIED. ) ;
#8138 = CARTESIAN_POINT ( 'NONE',  ( 0.2341512108694265570, -0.2669480828848097009, 1.953740157480315043 ) ) ;
#8139 = ORIENTED_EDGE ( 'NONE', *, *, #15121, .T. ) ;
#8140 = ORIENTED_EDGE ( 'NONE', *, *, #22856, .F. ) ;
#8141 = ADVANCED_FACE ( 'NONE', ( #6275 ), #18972, .T. ) ;
#8142 = AXIS2_PLACEMENT_3D ( 'NONE', #9186, #16129, #22476 ) ;
#8143 = CARTESIAN_POINT ( 'NONE',  ( -0.6020026763137992232, -0.1224252381418852453, -0.2454157907868443067 ) ) ;
#8144 = CARTESIAN_POINT ( 'NONE',  ( 0.1490609433615240342, -0.2393035190771456711, 0.4144858534716441278 ) ) ;
#8146 = CARTESIAN_POINT ( 'NONE',  ( -0.4539000224941007744, 0.3482225189667277343, 0.9399606299212598381 ) ) ;
#8145 = CARTESIAN_POINT ( 'NONE',  ( -1.456051859514965975E-17, 0.4692913385826771866, 0.1992150590373740204 ) ) ;
#8147 = EDGE_LOOP ( 'NONE', ( #2003, #21102, #8346, #9123 ) ) ;
#8148 = CARTESIAN_POINT ( 'NONE',  ( -0.4055118110236220486, 0.9448818897637796255, -9.561468503937007847E-18 ) ) ;
#8149 = DIRECTION ( 'NONE',  ( 0.000000000000000000, 0.000000000000000000, -1.000000000000000000 ) ) ;
#8150 = ADVANCED_FACE ( 'NONE', ( #19776 ), #12758, .T. ) ;
#8151 = EDGE_CURVE ( 'NONE', #15134, #8851, #8248, .T. ) ;
#8152 = DIRECTION ( 'NONE',  ( 0.000000000000000000, 1.000000000000000000, 0.000000000000000000 ) ) ;
#8153 = CARTESIAN_POINT ( 'NONE',  ( 0.3905379133858267737, 0.2805118110236220486, 0.4858607088160724063 ) ) ;
#8154 = DIRECTION ( 'NONE',  ( 0.000000000000000000, 0.000000000000000000, 1.000000000000000000 ) ) ;
#8155 = EDGE_CURVE ( 'NONE', #15191, #14962, #24958, .T. ) ;
#8156 = DIRECTION ( 'NONE',  ( 0.000000000000000000, -0.9999999999742198442, -7.180547322999998243E-06 ) ) ;
#8157 = CARTESIAN_POINT ( 'NONE',  ( 0.3209354104558860277, 0.3834063931588274077, 0.1496602734615972985 ) ) ;
#8158 = EDGE_CURVE ( 'NONE', #14933, #14153, #6793, .T. ) ;
#8159 = CARTESIAN_POINT ( 'NONE',  ( 0.3429980251342297226, -0.09187177619658888628, 1.953740157480315043 ) ) ;
#8160 = EDGE_CURVE ( 'NONE', #3201, #12475, #23519, .T. ) ;
#8161 = VERTEX_POINT ( 'NONE', #26269 ) ;
#8162 = CARTESIAN_POINT ( 'NONE',  ( -0.6707652279343347956, -0.1538768215240151616, 0.3401574803149606252 ) ) ;
#8163 = CIRCLE ( 'NONE', #23504, 0.1181102362204724532 ) ;
#8164 = DIRECTION ( 'NONE',  ( 1.000000000000000000, 0.000000000000000000, 0.000000000000000000 ) ) ;
#8165 = DIRECTION ( 'NONE',  ( 1.000000000000000000, 0.000000000000000000, 0.000000000000000000 ) ) ;
#8166 = CARTESIAN_POINT ( 'NONE',  ( -0.4165721057576322606, 0.3313508221749649763, 0.3401574803149606252 ) ) ;
#8167 = CARTESIAN_POINT ( 'NONE',  ( -0.3015429802557554329, -0.1746717017760298918, 0.1166443193911902154 ) ) ;
#8168 = CARTESIAN_POINT ( 'NONE',  ( 0.4856708409200598542, 0.1649135259617023896, 1.747047244094488194 ) ) ;
#8169 = ORIENTED_EDGE ( 'NONE', *, *, #373, .T. ) ;
#8170 = ORIENTED_EDGE ( 'NONE', *, *, #7921, .T. ) ;
#8171 = CARTESIAN_POINT ( 'NONE',  ( -2.685748425196850164E-17, 0.000000000000000000, -3.666338582670846780 ) ) ;
#8172 = ORIENTED_EDGE ( 'NONE', *, *, #8358, .F. ) ;
#8173 = CARTESIAN_POINT ( 'NONE',  ( -0.1658689444494333143, -0.4574452598450142737, 0.09284957166512360083 ) ) ;
#8174 = SHAPE_REPRESENTATION_RELATIONSHIP ( 'NONE' , 'NONE' ,  #6338, #922 ) ;
#8175 = CARTESIAN_POINT ( 'NONE',  ( 0.1677079028045456166, 0.2904160862623617056, 1.973425196850393970 ) ) ;
#8176 = ORIENTED_EDGE ( 'NONE', *, *, #26211, .T. ) ;
#8177 = CARTESIAN_POINT ( 'NONE',  ( -0.2180862235769436830, 0.4423390553432706707, -1.550196850393700920 ) ) ;
#8178 = CARTESIAN_POINT ( 'NONE',  ( 4.821444091131312140E-17, 0.8661417322803149910, 0.3937007874015748254 ) ) ;
#8179 = ORIENTED_EDGE ( 'NONE', *, *, #2570, .F. ) ;
#8180 = ORIENTED_EDGE ( 'NONE', *, *, #8214, .F. ) ;
#8181 = EDGE_CURVE ( 'NONE', #24304, #6563, #17653, .T. ) ;
#8182 = VECTOR ( 'NONE', #20130, 39.37007874015748854 ) ;
#8183 = ITEM_DEFINED_TRANSFORMATION ( 'NONE', 'NONE', #744,  #11588 ) ;
#8184 = CARTESIAN_POINT ( 'NONE',  ( -0.3529960615022087467, 0.06172929298840394013, 0.1805249803415331367 ) ) ;
#8185 = CARTESIAN_POINT ( 'NONE',  ( -0.0005696707463070112927, 0.4606295689977898400, 0.1771653543307085965 ) ) ;
#8186 = CARTESIAN_POINT ( 'NONE',  ( 0.1522836969735573143, 0.4909267390297480382, 0.05591742528025173131 ) ) ;
#8187 = FACE_OUTER_BOUND ( 'NONE', #22720, .T. ) ;
#8188 = EDGE_CURVE ( 'NONE', #27673, #5084, #27682, .T. ) ;
#8189 = ORIENTED_EDGE ( 'NONE', *, *, #26368, .F. ) ;
#8190 = EDGE_CURVE ( 'NONE', #8124, #14678, #9076, .T. ) ;
#8191 = DIRECTION ( 'NONE',  ( 0.000000000000000000, 0.000000000000000000, 1.000000000000000000 ) ) ;
#8192 = CARTESIAN_POINT ( 'NONE',  ( 4.821444091131312140E-17, 0.5905511811023621549, 0.3937007874015748254 ) ) ;
#8193 = DIRECTION ( 'NONE',  ( -1.000000000000000000, 0.000000000000000000, 0.000000000000000000 ) ) ;
#8194 = DIRECTION ( 'NONE',  ( 0.7071067811865480168, -0.7071067811865470176, 0.000000000000000000 ) ) ;
#8195 = AXIS2_PLACEMENT_3D ( 'NONE', #16866, #2016, #13030 ) ;
#8196 = CARTESIAN_POINT ( 'NONE',  ( -0.4621951630817676682, 0.08130208312401832060, 0.07637549214372854611 ) ) ;
#8197 = CARTESIAN_POINT ( 'NONE',  ( -0.09842519685039370636, -5.111401574803149519E-18, 0.000000000000000000 ) ) ;
#8198 = CARTESIAN_POINT ( 'NONE',  ( -0.6205631318075456315, -0.4724394499398413827, -0.9954595798869798617 ) ) ;
#8199 = DIRECTION ( 'NONE',  ( 0.000000000000000000, 0.000000000000000000, -1.000000000000000000 ) ) ;
#8200 = VECTOR ( 'NONE', #13359, 39.37007874015748143 ) ;
#8201 = DIRECTION ( 'NONE',  ( -0.000000000000000000, -1.000000000000000000, -0.000000000000000000 ) ) ;
#8202 = ORIENTED_EDGE ( 'NONE', *, *, #1809, .F. ) ;
#8203 = CARTESIAN_POINT ( 'NONE',  ( 0.6241887519799542705, 0.3029073140874565251, -0.5246508579836989261 ) ) ;
#8204 = CARTESIAN_POINT ( 'NONE',  ( 0.4232283464566928832, 0.000000000000000000, 0.1377952755905511861 ) ) ;
#8205 = ( NAMED_UNIT ( * ) PLANE_ANGLE_UNIT ( ) SI_UNIT ( $, .RADIAN. ) ) ;
#8206 = ORIENTED_EDGE ( 'NONE', *, *, #17821, .F. ) ;
#8207 = CARTESIAN_POINT ( 'NONE',  ( -0.5118110236220473341, 0.000000000000000000, -1.550196850393700920 ) ) ;
#8208 = DIRECTION ( 'NONE',  ( 1.000000000000000000, 0.000000000000000000, 0.000000000000000000 ) ) ;
#8209 = DIRECTION ( 'NONE',  ( -1.000000000000000000, 0.000000000000000000, 0.000000000000000000 ) ) ;
#8210 = ORIENTED_EDGE ( 'NONE', *, *, #5327, .T. ) ;
#8211 = EDGE_CURVE ( 'NONE', #24915, #5352, #12624, .T. ) ;
#8212 = CARTESIAN_POINT ( 'NONE',  ( 0.2420394123212937232, 0.2892587550802425134, 0.07637795275590551769 ) ) ;
#8213 = ORIENTED_EDGE ( 'NONE', *, *, #24514, .T. ) ;
#8214 = EDGE_CURVE ( 'NONE', #21688, #16430, #5025, .T. ) ;
#8215 = DIRECTION ( 'NONE',  ( 0.000000000000000000, -1.000000000000000000, 0.000000000000000000 ) ) ;
#8216 = CIRCLE ( 'NONE', #5511, 0.1771653543307086798 ) ;
#8217 = CARTESIAN_POINT ( 'NONE',  ( -0.0005789221761214173069, 0.4692909815006417462, 0.07637795275590551769 ) ) ;
#8218 = DIRECTION ( 'NONE',  ( 1.000000000000000000, 0.000000000000000000, 0.000000000000000000 ) ) ;
#8219 = DIRECTION ( 'NONE',  ( 0.000000000000000000, 0.000000000000000000, -1.000000000000000000 ) ) ;
#8220 = VERTEX_POINT ( 'NONE', #9641 ) ;
#8221 = CARTESIAN_POINT ( 'NONE',  ( 0.000000000000000000, 0.000000000000000000, -0.2618110236220472231 ) ) ;
#8222 = CARTESIAN_POINT ( 'NONE',  ( 0.5484420430273854175, -0.3174147232949027786, 0.2481708550944002056 ) ) ;
#8223 = ORIENTED_EDGE ( 'NONE', *, *, #19267, .T. ) ;
#8224 = CARTESIAN_POINT ( 'NONE',  ( 0.2660793235464301021, -0.2041304421298313909, 1.973425196850393970 ) ) ;
#8225 = CARTESIAN_POINT ( 'NONE',  ( 0.4856708409191422549, -0.1649135259639211148, -1.550196850393700920 ) ) ;
#8226 = CARTESIAN_POINT ( 'NONE',  ( -0.03532354024591775193, -0.6299212598425196763, 0.000000000000000000 ) ) ;
#8227 = CARTESIAN_POINT ( 'NONE',  ( 0.2762247810518927427, -0.4783323773986943306, 0.9399606299212598381 ) ) ;
#8228 = CARTESIAN_POINT ( 'NONE',  ( 0.5393700787401575214, 0.000000000000000000, 0.2637795275590551491 ) ) ;
#8229 = ORIENTED_EDGE ( 'NONE', *, *, #12797, .F. ) ;
#8230 = B_SPLINE_SURFACE_WITH_KNOTS ( 'NONE', 2, 3, ( 
 ( #4567, #23426, #24060, #13321, #6833, #17687, #27792, #1929, #6318, #14949, #2573, #17570, #26311, #6976, #13448, #26438, #2705, #11338, #24326, #2838, #19955, #4975, #13588, #5254, #24741, #9623, #20514, #26574, #22921, #891, #1172, #16282, #20793, #18074, #13875, #18366, #17941, #26718, #3394, #20231, #14169, #2976, #5104, #20653, #24885, #22493, #3255, #3123, #27019, #9771, #16412, #1305, #27162, #22632, #22769, #12037, #9914, #18514, #9478, #15999, #24453, #11750, #7806, #5403, #11895, #25027 ),
 ( #5691, #3540, #20371, #12168, #7232, #9335, #13729, #22351, #1029, #14021, #18227, #26865, #7517, #8373, #14756, #25457, #27865, #12602, #4129, #3686, #10182, #16986, #21223, #23209, #25598, #14608, #17122, #21363, #8502, #15018, #23498, #12734, #25739, #6391, #3841, #1580, #19234, #23633, #1865, #10470, #27295, #5835, #19088, #8227, #18656, #27586, #12315, #21070, #8090, #7946, #16847, #1719, #18801, #2000, #27436, #10331, #12874, #10049, #20936, #1438, #23363, #16547, #16703, #6254, #25165, #18951 ),
 ( #23068, #6121, #27727, #14459, #3987, #14889, #10611, #25314, #5973, #2274, #8772, #21503, #332, #19663, #11038, #15436, #4406, #4946, #15693, #13012, #17534, #6526, #4666, #6804, #24296, #13417, #15158, #17261, #4802, #26411, #19516, #22044, #26014, #17395, #26149, #21776, #13294, #10758, #7077, #21643, #21917, #19790, #2143, #10898, #6669, #2544, #74, #205, #15567, #23767, #26279, #15301, #25879, #2678, #453, #23907, #24027, #4545, #11170, #9044, #579, #11307, #19926, #17658, #6945, #24167 ) ),
 .UNSPECIFIED., .F., .T., .F.,
 ( 3, 3 ),
 ( 4, 2, 2, 2, 2, 2, 2, 2, 2, 2, 2, 2, 2, 2, 2, 2, 2, 2, 2, 2, 2, 2, 2, 2, 2, 2, 2, 2, 2, 2, 2, 2, 4 ),
 ( 0.000000000000000000, 1.000000000000000000 ),
 ( 0.000000000000000000, 0.1963495408493620697, 0.3926990816987241395, 0.5890486225480862092, 0.7853981633974482790, 0.9817477042468103487, 1.178097245096172418, 1.374446785945534488, 1.570796326794896558, 1.767145867644258628, 1.963495408493620697, 2.159844949342982545, 2.356194490192344837, 2.552544031041707129, 2.748893571891068976, 2.945243112740430824, 3.141592653589793116, 3.337942194439155408, 3.534291735288517255, 3.730641276137879103, 3.926990816987241395, 4.123340357836603687, 4.319689898685965090, 4.516039439535327382, 4.712388980384689674, 4.908738521234051966, 5.105088062083414258, 5.301437602932775661, 5.497787143782137953, 5.694136684631500245, 5.890486225480861648, 6.086835766330223940, 6.283185307179586232 ),
 .UNSPECIFIED. ) ;
#8231 = CARTESIAN_POINT ( 'NONE',  ( 0.1516263115863346334, -0.1971492568089271424, 0.4530651079966787620 ) ) ;
#8232 = AXIS2_PLACEMENT_3D ( 'NONE', #13199, #21829, #19708 ) ;
#8233 = TOROIDAL_SURFACE ( 'NONE', #18587, 0.6102362204724409711, 0.1299212598425196763 ) ;
#8234 = CARTESIAN_POINT ( 'NONE',  ( 0.5280918803863992039, 0.06946904943156809176, 1.747047244094488860 ) ) ;
#8235 = ORIENTED_EDGE ( 'NONE', *, *, #9210, .T. ) ;
#8236 = AXIS2_PLACEMENT_3D ( 'NONE', #2607, #11230, #924 ) ;
#8237 = CARTESIAN_POINT ( 'NONE',  ( -0.5085118447796660446, 0.06699507805605008082, -1.550196850393700920 ) ) ;
#8238 = ORIENTED_EDGE ( 'NONE', *, *, #22758, .T. ) ;
#8239 = DIRECTION ( 'NONE',  ( 0.000000000000000000, 1.000000000000000000, 0.000000000000000000 ) ) ;
#8240 = CARTESIAN_POINT ( 'NONE',  ( -0.3715251363271980245, 0.06498290224717540031, 0.07637795275590551769 ) ) ;
#8241 = CARTESIAN_POINT ( 'NONE',  ( 0.000000000000000000, 0.000000000000000000, 0.01181102362204724393 ) ) ;
#8242 = CARTESIAN_POINT ( 'NONE',  ( 0.1379032889623779401, -0.5144765700550301135, 1.747047244094488194 ) ) ;
#8243 = EDGE_CURVE ( 'NONE', #11425, #4356, #23553, .T. ) ;
#8244 = CARTESIAN_POINT ( 'NONE',  ( 0.000000000000000000, 0.07874015748662489822, -0.2952755905511805778 ) ) ;
#8245 = ORIENTED_EDGE ( 'NONE', *, *, #675, .T. ) ;
#8246 = CARTESIAN_POINT ( 'NONE',  ( -0.09776456083825368903, 0.2994062042887761232, -3.259552405628561189 ) ) ;
#8247 = DIRECTION ( 'NONE',  ( -1.000000000000000000, 0.000000000000000000, 0.000000000000000000 ) ) ;
#8248 = LINE ( 'NONE', #14909, #25321 ) ;
#8249 = EDGE_LOOP ( 'NONE', ( #301, #23582, #13785, #6351 ) ) ;
#8250 = AXIS2_PLACEMENT_3D ( 'NONE', #19701, #24340, #2851 ) ;
#8251 = DIRECTION ( 'NONE',  ( 0.000000000000000000, 0.000000000000000000, 1.000000000000000000 ) ) ;
#8252 = VECTOR ( 'NONE', #10782, 39.37007874015748143 ) ;
#8253 = EDGE_LOOP ( 'NONE', ( #8318, #21304 ) ) ;
#8254 = CARTESIAN_POINT ( 'NONE',  ( 0.09842519685039370636, 0.2165354330708661457, -3.272637795275590733 ) ) ;
#8255 = FACE_OUTER_BOUND ( 'NONE', #17710, .T. ) ;
#8256 = CARTESIAN_POINT ( 'NONE',  ( -0.4121342552748409327, 0.2031943647053852109, -1.928289503579154074 ) ) ;
#8257 = AXIS2_PLACEMENT_3D ( 'NONE', #12312, #1717, #12461 ) ;
#8258 = CARTESIAN_POINT ( 'NONE',  ( -0.3334645669291338987, 1.279353152430305007, -0.8465078874097147210 ) ) ;
#8259 = ADVANCED_FACE ( 'NONE', ( #27115 ), #7901, .F. ) ;
#8260 = EDGE_CURVE ( 'NONE', #17635, #4182, #8805, .T. ) ;
#8261 = EDGE_LOOP ( 'NONE', ( #25645, #20342, #3086, #16725, #18542, #10519 ) ) ;
#8262 = ORIENTED_EDGE ( 'NONE', *, *, #20508, .F. ) ;
#8263 = CARTESIAN_POINT ( 'NONE',  ( -0.6002615430280354714, -0.1750105204655757751, 0.06519039343118070151 ) ) ;
#8264 = DIRECTION ( 'NONE',  ( -0.3420201433256691570, 0.9396926207859084279, 0.000000000000000000 ) ) ;
#8265 = ITEM_DEFINED_TRANSFORMATION ( 'NONE', 'NONE', #22897,  #11588 ) ;
#8266 = ORIENTED_EDGE ( 'NONE', *, *, #20313, .F. ) ;
#8267 = CARTESIAN_POINT ( 'NONE',  ( 0.000000000000000000, 0.000000000000000000, -0.2618110236220472231 ) ) ;
#8268 = AXIS2_PLACEMENT_3D ( 'NONE', #23977, #15389, #13236 ) ;
#8269 = ORIENTED_EDGE ( 'NONE', *, *, #875, .T. ) ;
#8270 = CONICAL_SURFACE ( 'NONE', #14140, 0.06200787401574806013, 0.5235987755983000369 ) ;
#8271 = DIRECTION ( 'NONE',  ( 1.000000000000000000, 0.000000000000000000, 0.000000000000000000 ) ) ;
#8272 = CARTESIAN_POINT ( 'NONE',  ( -0.4535326485287287657, 0.08054850140359764987, 0.1771653543307088186 ) ) ;
#8273 = EDGE_CURVE ( 'NONE', #15380, #10004, #23976, .T. ) ;
#8274 = CARTESIAN_POINT ( 'NONE',  ( 0.4210617728748768385, -0.2437762437830508222, 0.2467937632988287666 ) ) ;
#8275 = CIRCLE ( 'NONE', #22260, 0.3180687940323247975 ) ;
#8276 = CARTESIAN_POINT ( 'NONE',  ( 0.000000000000000000, 0.4724409448818898127, 0.000000000000000000 ) ) ;
#8277 = ORIENTED_EDGE ( 'NONE', *, *, #2268, .F. ) ;
#8278 = CARTESIAN_POINT ( 'NONE',  ( -0.2341512108694372152, -0.2669480828848191933, 1.953740157480315043 ) ) ;
#8279 = ORIENTED_EDGE ( 'NONE', *, *, #6435, .T. ) ;
#8280 = AXIS2_PLACEMENT_3D ( 'NONE', #23766, #6524, #21641 ) ;
#8281 = CARTESIAN_POINT ( 'NONE',  ( -0.5688514329716306550, -0.1961983850004131169, -0.2600699532609946907 ) ) ;
#8282 = CARTESIAN_POINT ( 'NONE',  ( -0.5376957092749378164, -0.3112026930392873814, 0.2574803149606298969 ) ) ;
#8283 = CARTESIAN_POINT ( 'NONE',  ( 0.4066108233583488052, -0.2343118354750409471, 0.1992142434433716580 ) ) ;
#8284 = AXIS2_PLACEMENT_3D ( 'NONE', #1135, #26681, #18041 ) ;
#8285 = LINE ( 'NONE', #13070, #13513 ) ;
#8286 = B_SPLINE_CURVE_WITH_KNOTS ( 'NONE', 3,
 ( #15969, #24571, #24994, #22893, #12011, #14578 ),
 .UNSPECIFIED., .F., .F.,
 ( 4, 2, 4 ),
 ( 0.7157687286427130147, 0.7172350147555660582, 0.7187013008684189908 ),
 .UNSPECIFIED. ) ;
#8287 = ORIENTED_EDGE ( 'NONE', *, *, #22387, .T. ) ;
#8288 = DIRECTION ( 'NONE',  ( 1.224646799147353207E-16, 1.000000000000000000, -0.000000000000000000 ) ) ;
#8289 = FACE_OUTER_BOUND ( 'NONE', #4025, .T. ) ;
#8290 = CARTESIAN_POINT ( 'NONE',  ( 0.3460635936744816399, 0.09269288654273792616, -3.115157480314960647 ) ) ;
#8291 = CARTESIAN_POINT ( 'NONE',  ( 6.136516277395897527E-17, 0.2165354330708661457, -3.646653543307086576 ) ) ;
#8292 = DIRECTION ( 'NONE',  ( -1.000000000000000000, 0.000000000000000000, 0.000000000000000000 ) ) ;
#8293 = CARTESIAN_POINT ( 'NONE',  ( 0.1518453843511950729, 0.1971119371026649747, 0.4530813475000622370 ) ) ;
#8294 = AXIS2_PLACEMENT_3D ( 'NONE', #5257, #16145, #9626 ) ;
#8295 = DIRECTION ( 'NONE',  ( 0.000000000000000000, 0.000000000000000000, 1.000000000000000000 ) ) ;
#8296 = EDGE_CURVE ( 'NONE', #9494, #3772, #13594, .T. ) ;
#8297 = CARTESIAN_POINT ( 'NONE',  ( -0.5811930530674194184, -0.4724394499398544278, -0.9954595798869386725 ) ) ;
#8298 = CARTESIAN_POINT ( 'NONE',  ( 0.3362336590883814313, -0.1141709026133623794, 1.953740157480315043 ) ) ;
#8299 = ORIENTED_EDGE ( 'NONE', *, *, #24446, .T. ) ;
#8300 = CARTESIAN_POINT ( 'NONE',  ( 0.000000000000000000, 0.000000000000000000, 0.01181102362204724393 ) ) ;
#8301 = CARTESIAN_POINT ( 'NONE',  ( -0.0005696707463066808278, 0.4606295689977896735, 0.1639447408835300324 ) ) ;
#8302 = AXIS2_PLACEMENT_3D ( 'NONE', #16921, #25531, #10123 ) ;
#8303 = ORIENTED_EDGE ( 'NONE', *, *, #13257, .F. ) ;
#8304 = EDGE_LOOP ( 'NONE', ( #11579, #14620 ) ) ;
#8305 = VECTOR ( 'NONE', #27497, 39.37007874015748143 ) ;
#8306 = ORIENTED_EDGE ( 'NONE', *, *, #10189, .F. ) ;
#8307 = CARTESIAN_POINT ( 'NONE',  ( -0.5677441908128973980, 0.3966471237414492257, -0.3366160073295133004 ) ) ;
#8308 = CARTESIAN_POINT ( 'NONE',  ( 0.08600259727896249207, 0.2165354330708661457, -3.597797143737292647 ) ) ;
#8309 = CARTESIAN_POINT ( 'NONE',  ( -0.2952755905264887182, 3.616083068046089993E-17, -4.330708661417323135 ) ) ;
#8310 = ADVANCED_FACE ( 'NONE', ( #9361, #13755 ), #16170, .T. ) ;
#8311 = VERTEX_POINT ( 'NONE', #5429 ) ;
#8312 = ORIENTED_EDGE ( 'NONE', *, *, #3343, .T. ) ;
#8313 = CARTESIAN_POINT ( 'NONE',  ( 0.2842490391651530390, 0.2180698645301770711, -3.115157480314960647 ) ) ;
#8314 = ADVANCED_FACE ( 'NONE', ( #4855, #18397 ), #22099, .T. ) ;
#8315 = CARTESIAN_POINT ( 'NONE',  ( -0.1694923354741917354, -0.4674199084399158766, 0.1615162260944750239 ) ) ;
#8316 = CIRCLE ( 'NONE', #27716, 0.01181102362204724046 ) ;
#8317 = CARTESIAN_POINT ( 'NONE',  ( 0.2904160862623596517, -0.1677079028045486975, 1.973425196850393970 ) ) ;
#8318 = ORIENTED_EDGE ( 'NONE', *, *, #18492, .F. ) ;
#8319 = ORIENTED_EDGE ( 'NONE', *, *, #5981, .T. ) ;
#8320 = CARTESIAN_POINT ( 'NONE',  ( 0.4921259842519685179, -0.03220957031753991784, -1.550196850393700920 ) ) ;
#8321 = CARTESIAN_POINT ( 'NONE',  ( 0.000000000000000000, 0.3937007874015748254, 0.4488188976377953110 ) ) ;
#8322 = ORIENTED_EDGE ( 'NONE', *, *, #13018, .F. ) ;
#8323 = ORIENTED_EDGE ( 'NONE', *, *, #7982, .T. ) ;
#8324 = AXIS2_PLACEMENT_3D ( 'NONE', #721, #22047, #4546 ) ;
#8325 = B_SPLINE_CURVE_WITH_KNOTS ( 'NONE', 3,
 ( #24728, #13716, #5391, #11597, #882, #7793, #27423, #3529, #1293, #25300 ),
 .UNSPECIFIED., .F., .F.,
 ( 4, 2, 2, 2, 4 ),
 ( 0.000000000000000000, 0.2499999999999997780, 0.5000000000000000000, 0.7500000000000002220, 1.000000000000000000 ),
 .UNSPECIFIED. ) ;
#8326 = ITEM_DEFINED_TRANSFORMATION ( 'NONE', 'NONE', #21052,  #11588 ) ;
#8327 = DIRECTION ( 'NONE',  ( 0.000000000000000000, 0.000000000000000000, 1.000000000000000000 ) ) ;
#8328 = AXIS2_PLACEMENT_3D ( 'NONE', #3705, #15811, #7621 ) ;
#8329 = DIRECTION ( 'NONE',  ( 0.6427876096865391409, -0.7660444431189782355, 0.000000000000000000 ) ) ;
#8330 = CARTESIAN_POINT ( 'NONE',  ( -0.3198827364362346048, 0.000000000000000000, -0.1725236688546921415 ) ) ;
#8331 = ORIENTED_EDGE ( 'NONE', *, *, #23563, .T. ) ;
#8332 = CARTESIAN_POINT ( 'NONE',  ( 0.1495939273659548374, -0.2199999812874746663, -0.4279560700802453321 ) ) ;
#8333 = FACE_OUTER_BOUND ( 'NONE', #1815, .T. ) ;
#8334 = ADVANCED_BREP_SHAPE_REPRESENTATION ( 'Output Shaft', ( #21369, #11588 ), #26943 ) ;
#8335 = AXIS2_PLACEMENT_3D ( 'NONE', #16519, #3513, #1405 ) ;
#8336 = CARTESIAN_POINT ( 'NONE',  ( 0.7874015748031496509, 0.000000000000000000, 0.2362204724409449619 ) ) ;
#8337 = DIRECTION ( 'NONE',  ( 0.000000000000000000, 0.000000000000000000, -1.000000000000000000 ) ) ;
#8338 = ADVANCED_FACE ( 'NONE', ( #7692 ), #12699, .T. ) ;
#8339 = CARTESIAN_POINT ( 'NONE',  ( -0.4325335578080637955, -0.8196558064895489437, -0.05799776393766782612 ) ) ;
#8340 = CARTESIAN_POINT ( 'NONE',  ( 0.4006498629591506155, 0.2309201403895323190, -1.928289503579156960 ) ) ;
#8341 = CARTESIAN_POINT ( 'NONE',  ( 0.3722026523000413478, 4.558167867734008572E-17, -0.05856299212598425896 ) ) ;
#8342 = DIRECTION ( 'NONE',  ( -1.000000000000000000, 0.000000000000000000, 0.000000000000000000 ) ) ;
#8343 = EDGE_CURVE ( 'NONE', #4773, #12691, #18062, .T. ) ;
#8344 = CARTESIAN_POINT ( 'NONE',  ( 0.09586345222254785692, 0.1968503937007873850, -3.246875207736358515 ) ) ;
#8345 = CARTESIAN_POINT ( 'NONE',  ( 4.821444091131312140E-17, 0.8661417322803149910, 0.3937007874015748254 ) ) ;
#8346 = ORIENTED_EDGE ( 'NONE', *, *, #45, .F. ) ;
#8347 = AXIS2_PLACEMENT_3D ( 'NONE', #17181, #8292, #23693 ) ;
#8348 = ORIENTED_EDGE ( 'NONE', *, *, #16773, .F. ) ;
#8349 = CARTESIAN_POINT ( 'NONE',  ( 0.000000000000000000, 0.09092130223458683158, -0.3779527559055118058 ) ) ;
#8350 = CARTESIAN_POINT ( 'NONE',  ( 0.1288360683667812978, -0.3544784926413476200, 0.07637549214372835182 ) ) ;
#8351 = ORIENTED_EDGE ( 'NONE', *, *, #2760, .F. ) ;
#8352 = DIRECTION ( 'NONE',  ( 0.000000000000000000, 0.000000000000000000, 1.000000000000000000 ) ) ;
#8353 = CARTESIAN_POINT ( 'NONE',  ( -0.4029514798614846072, 0.3205030004507355978, 0.1473214333197954140 ) ) ;
#8354 = DIRECTION ( 'NONE',  ( 1.000000000000000000, 0.000000000000000000, 0.000000000000000000 ) ) ;
#8355 = ORIENTED_EDGE ( 'NONE', *, *, #17101, .F. ) ;
#8356 = AXIS2_PLACEMENT_3D ( 'NONE', #136, #10829, #25534 ) ;
#8357 = EDGE_LOOP ( 'NONE', ( #13425, #7835 ) ) ;
#8358 = EDGE_CURVE ( 'NONE', #17275, #12205, #15228, .T. ) ;
#8359 = CARTESIAN_POINT ( 'NONE',  ( 0.5377323685532543474, 0.4294741335735771659, 0.3401591245381551110 ) ) ;
#8360 = CARTESIAN_POINT ( 'NONE',  ( -0.0005847768872542869270, 0.4787829797961313250, 0.08349695147752332625 ) ) ;
#8361 = LINE ( 'NONE', #19366, #7785 ) ;
#8362 = CIRCLE ( 'NONE', #25940, 0.4921259842519685179 ) ;
#8363 = CARTESIAN_POINT ( 'NONE',  ( -0.5314960629921260393, 6.402768735150616610E-17, 1.747047244094488194 ) ) ;
#8364 = VERTEX_POINT ( 'NONE', #20677 ) ;
#8365 = DIRECTION ( 'NONE',  ( 0.000000000000000000, 1.000000000000000000, 0.000000000000000000 ) ) ;
#8366 = CARTESIAN_POINT ( 'NONE',  ( -0.07874015748031495954, 0.1968503937007873850, -3.456364829396327831 ) ) ;
#8367 = AXIS2_PLACEMENT_3D ( 'NONE', #19784, #4793, #2676 ) ;
#8368 = ORIENTED_EDGE ( 'NONE', *, *, #4204, .T. ) ;
#8369 = DIRECTION ( 'NONE',  ( 1.000000000000000000, 0.000000000000000000, 0.000000000000000000 ) ) ;
#8370 = DIRECTION ( 'NONE',  ( 0.000000000000000000, 1.000000000000000000, 0.000000000000000000 ) ) ;
#8371 = FACE_OUTER_BOUND ( 'NONE', #10504, .T. ) ;
#8372 = EDGE_CURVE ( 'NONE', #19458, #23913, #12253, .T. ) ;
#8373 = CARTESIAN_POINT ( 'NONE',  ( -0.1775991818008579581, 0.5230301363771275858, 0.9399606299212598381 ) ) ;
#8374 = CARTESIAN_POINT ( 'NONE',  ( 0.000000000000000000, 0.4232283464566928832, -3.341531889763779686E-17 ) ) ;
#8375 = EDGE_LOOP ( 'NONE', ( #3342, #15180, #5615, #14706 ) ) ;
#8376 = CARTESIAN_POINT ( 'NONE',  ( 0.5905511811023621549, 0.000000000000000000, 0.000000000000000000 ) ) ;
#8377 = EDGE_CURVE ( 'NONE', #17187, #21448, #16721, .T. ) ;
#8378 = VERTEX_POINT ( 'NONE', #12623 ) ;
#8379 = VECTOR ( 'NONE', #7240, 39.37007874015748143 ) ;
#8380 = CARTESIAN_POINT ( 'NONE',  ( 0.2564944395535760924, 0.4441657790094617475, -1.550196850393700920 ) ) ;
#8381 = DIRECTION ( 'NONE',  ( 0.000000000000000000, 1.000000000000000000, 0.000000000000000000 ) ) ;
#8382 = AXIS2_PLACEMENT_3D ( 'NONE', #24697, #7545, #16174 ) ;
#8383 = CARTESIAN_POINT ( 'NONE',  ( -1.466875984251968630E-17, 0.000000000000000000, -0.4566929133858267376 ) ) ;
#8384 = CARTESIAN_POINT ( 'NONE',  ( 1.857656692913385893E-16, 0.000000000000000000, 0.000000000000000000 ) ) ;
#8385 = CARTESIAN_POINT ( 'NONE',  ( 0.09590060490395689585, 0.1136516277932334562, 0.1968503937007874127 ) ) ;
#8386 = CARTESIAN_POINT ( 'NONE',  ( -0.5744829134145985616, -0.4891471943182150173, 0.9948696824535705474 ) ) ;
#8387 = ORIENTED_EDGE ( 'NONE', *, *, #8190, .T. ) ;
#8388 = EDGE_CURVE ( 'NONE', #21046, #2655, #25189, .T. ) ;
#8389 = TOROIDAL_SURFACE ( 'NONE', #13796, 0.4232283464566928832, 0.07677165354330708902 ) ;
#8390 = CARTESIAN_POINT ( 'NONE',  ( -0.6169742724477221829, -0.4807970751196540271, -0.9954635886630591735 ) ) ;
#8391 = LINE ( 'NONE', #7968, #11283 ) ;
#8392 = CARTESIAN_POINT ( 'NONE',  ( -0.3715251363271980245, 0.06498290224717540031, 0.07637795275590551769 ) ) ;
#8393 = CARTESIAN_POINT ( 'NONE',  ( 0.1658689444493339771, -0.4574452598447248941, 0.09284957166472920798 ) ) ;
#8394 = CIRCLE ( 'NONE', #22823, 0.5322834645669292097 ) ;
#8395 = CARTESIAN_POINT ( 'NONE',  ( -0.5905511811023621549, 0.9448818897637796255, -1.639108661417322569E-17 ) ) ;
#8396 = PLANE ( 'NONE',  #5082 ) ;
#8397 = EDGE_LOOP ( 'NONE', ( #21774, #14914, #4827, #3222, #26384, #25952 ) ) ;
#8398 = CARTESIAN_POINT ( 'NONE',  ( -0.4921259842519685179, 0.000000000000000000, -1.569881889763779625 ) ) ;
#8399 = CARTESIAN_POINT ( 'NONE',  ( -0.2991932138496239402, -0.3411003281196705594, -1.934055118110236338 ) ) ;
#8400 = AXIS2_PLACEMENT_3D ( 'NONE', #6234, #8352, #25854 ) ;
#8401 = EDGE_CURVE ( 'NONE', #17480, #22690, #12236, .T. ) ;
#8402 = CIRCLE ( 'NONE', #19696, 0.3722026523000413478 ) ;
#8403 = ORIENTED_EDGE ( 'NONE', *, *, #16269, .T. ) ;
#8404 = ORIENTED_EDGE ( 'NONE', *, *, #13633, .T. ) ;
#8405 = CARTESIAN_POINT ( 'NONE',  ( -0.6068752646683485130, -0.1547367907410470145, 0.06814449279195373965 ) ) ;
#8406 = DIRECTION ( 'NONE',  ( 3.169619147893091460E-17, -0.9659258263664933786, 0.2588190448135661570 ) ) ;
#8407 = FACE_OUTER_BOUND ( 'NONE', #7318, .T. ) ;
#8408 = ORIENTED_EDGE ( 'NONE', *, *, #19019, .F. ) ;
#8409 = DIRECTION ( 'NONE',  ( 1.000000000000000000, 0.000000000000000000, 0.000000000000000000 ) ) ;
#8410 = DIRECTION ( 'NONE',  ( 1.000000000000000000, 0.000000000000000000, 0.000000000000000000 ) ) ;
#8411 = CARTESIAN_POINT ( 'NONE',  ( -0.2602238532265429005, 0.000000000000000000, 0.2362204724409449064 ) ) ;
#8412 = ORIENTED_EDGE ( 'NONE', *, *, #13636, .F. ) ;
#8413 = CARTESIAN_POINT ( 'NONE',  ( -0.3429980251342298336, -0.09187177619659059324, 1.953740157480315043 ) ) ;
#8414 = ORIENTED_EDGE ( 'NONE', *, *, #4633, .T. ) ;
#8415 = CARTESIAN_POINT ( 'NONE',  ( -0.5692936381921454014, -0.3294684677441130360, 0.1461456498322906972 ) ) ;
#8416 = CARTESIAN_POINT ( 'NONE',  ( -0.6149721272769592684, -0.09366413789291816450, -0.2415914643636047077 ) ) ;
#8417 = CIRCLE ( 'NONE', #5256, 0.1023622047244094474 ) ;
#8418 = ORIENTED_EDGE ( 'NONE', *, *, #3109, .F. ) ;
#8419 = DIRECTION ( 'NONE',  ( 1.000000000000000000, 0.000000000000000000, 0.000000000000000000 ) ) ;
#8420 = CARTESIAN_POINT ( 'NONE',  ( -1.452994488188976472E-16, 0.3149606299212598381, -3.646653543307086576 ) ) ;
#8421 = EDGE_CURVE ( 'NONE', #19774, #15164, #5856, .T. ) ;
#8422 = AXIS2_PLACEMENT_3D ( 'NONE', #20534, #9792, #2853 ) ;
#8423 = CARTESIAN_POINT ( 'NONE',  ( 0.2807137536170459802, 0.2462256503456008716, -3.115157480314960647 ) ) ;
#8424 = CARTESIAN_POINT ( 'NONE',  ( 0.000000000000000000, 0.000000000000000000, 0.3425196850393700809 ) ) ;
#8425 = CARTESIAN_POINT ( 'NONE',  ( 0.000000000000000000, 0.000000000000000000, 0.4724409448818898127 ) ) ;
#8426 = CARTESIAN_POINT ( 'NONE',  ( 2.483043706975895149E-16, 0.4724409448818898127, 1.988188976448617584 ) ) ;
#8427 = CARTESIAN_POINT ( 'NONE',  ( -2.158159842519685212E-16, 0.7086614173228346081, 0.000000000000000000 ) ) ;
#8428 = CARTESIAN_POINT ( 'NONE',  ( 0.07874015748031495954, -0.04546065111729338803, -0.4724409448818898127 ) ) ;
#8429 = EDGE_CURVE ( 'NONE', #13907, #5352, #5941, .T. ) ;
#8430 = DIRECTION ( 'NONE',  ( 0.000000000000000000, 0.000000000000000000, 1.000000000000000000 ) ) ;
#8431 = FACE_OUTER_BOUND ( 'NONE', #11310, .T. ) ;
#8432 = CARTESIAN_POINT ( 'NONE',  ( -0.5708661417322834497, 0.03749087971309117417, 0.9399606299212597271 ) ) ;
#8433 = ORIENTED_EDGE ( 'NONE', *, *, #20611, .F. ) ;
#8434 = AXIS2_PLACEMENT_3D ( 'NONE', #18536, #1195, #27042 ) ;
#8435 = DIRECTION ( 'NONE',  ( 0.000000000000000000, 0.000000000000000000, 1.000000000000000000 ) ) ;
#8436 = ( NAMED_UNIT ( * ) SI_UNIT ( $, .STERADIAN. ) SOLID_ANGLE_UNIT ( ) ) ;
#8437 = PRODUCT_CONTEXT ( 'NONE', #17718, 'mechanical' ) ;
#8438 = CARTESIAN_POINT ( 'NONE',  ( -0.4856708409200606313, -0.1649135259617140470, 1.766732283464566899 ) ) ;
#8439 = ORIENTED_EDGE ( 'NONE', *, *, #2323, .T. ) ;
#8440 = ORIENTED_EDGE ( 'NONE', *, *, #11042, .T. ) ;
#8441 = VERTEX_POINT ( 'NONE', #10205 ) ;
#8442 = CARTESIAN_POINT ( 'NONE',  ( -0.06002032661671168751, -0.4585215200179056372, -1.928289503579156516 ) ) ;
#8443 = CARTESIAN_POINT ( 'NONE',  ( 0.3149606299212598381, 0.000000000000000000, 0.000000000000000000 ) ) ;
#8444 = CARTESIAN_POINT ( 'NONE',  ( 0.08676778863010990717, 0.3239425792934408910, 1.973425196850393970 ) ) ;
#8445 = ORIENTED_EDGE ( 'NONE', *, *, #27546, .F. ) ;
#8446 = ORIENTED_EDGE ( 'NONE', *, *, #22416, .T. ) ;
#8447 = CARTESIAN_POINT ( 'NONE',  ( 0.2180862235769456536, -0.4423390553432768879, -1.550196850393700920 ) ) ;
#8448 = CARTESIAN_POINT ( 'NONE',  ( -0.4330708661417322913, -1.131889763779527547, 1.386165176200252194E-16 ) ) ;
#8449 = ORIENTED_EDGE ( 'NONE', *, *, #2784, .F. ) ;
#8450 = DIRECTION ( 'NONE',  ( -0.000000000000000000, 1.000000000000000000, 0.000000000000000000 ) ) ;
#8451 = EDGE_LOOP ( 'NONE', ( #8095, #26361, #25830, #21519, #13372, #6790, #725, #15217 ) ) ;
#8452 = ORIENTED_EDGE ( 'NONE', *, *, #15845, .T. ) ;
#8453 = ORIENTED_EDGE ( 'NONE', *, *, #15759, .T. ) ;
#8454 = DIRECTION ( 'NONE',  ( 1.000000000000000000, 0.000000000000000000, 0.000000000000000000 ) ) ;
#8455 = ( GEOMETRIC_REPRESENTATION_CONTEXT ( 3 ) GLOBAL_UNCERTAINTY_ASSIGNED_CONTEXT ( ( #857 ) ) GLOBAL_UNIT_ASSIGNED_CONTEXT ( ( #18780, #18205, #15975 ) ) REPRESENTATION_CONTEXT ( 'NONE', 'WORKASPACE' ) ) ;
#8456 = CARTESIAN_POINT ( 'NONE',  ( 0.4563908000639795848, 1.076366897322332816, -0.3413933471944003428 ) ) ;
#8457 = CARTESIAN_POINT ( 'NONE',  ( -0.006553447611498987302, 0.3149606299212598381, -3.646653543307087020 ) ) ;
#8458 = CARTESIAN_POINT ( 'NONE',  ( 0.1570092758121679200, -0.4330450457732857861, 0.1771653543307087630 ) ) ;
#8459 = ORIENTED_EDGE ( 'NONE', *, *, #17268, .F. ) ;
#8460 = B_SPLINE_SURFACE_WITH_KNOTS ( 'NONE', 2, 3, ( 
 ( #25708, #19207, #1447, #10732, #6359, #1972, #23877, #10582, #14993, #8881, #20800, #17499, #19480, #25986, #46, #2376, #23738, #6224 ),
 ( #15265, #11008, #8344, #27692, #306, #19346, #23607, #8609, #4373, #25847, #6497, #26120, #2243, #174, #17092, #10865, #27835, #15410 ),
 ( #8749, #23471, #10056, #4242, #17369, #12843, #18662, #16957, #25572, #14860, #12705, #21338, #8472, #2116, #4512, #13121, #9415, #13394 ) ),
 .UNSPECIFIED., .F., .F., .F.,
 ( 3, 3 ),
 ( 4, 2, 2, 2, 2, 2, 2, 2, 4 ),
 ( 0.000000000000000000, 1.000000000000000000 ),
 ( 1.570796326794896558, 1.963495408493620697, 2.356194490192344837, 2.748893571891068976, 3.141592653589793116, 3.534291735288517255, 3.926990816987241395, 4.319689898685965090, 4.712388980384689674 ),
 .UNSPECIFIED. ) ;
#8461 = ADVANCED_FACE ( 'NONE', ( #24908 ), #16873, .T. ) ;
#8462 = CARTESIAN_POINT ( 'NONE',  ( -0.4776900717921101491, 0.2356240016489475342, 1.747047244094488638 ) ) ;
#8463 = DIRECTION ( 'NONE',  ( -1.000000000000000000, 0.000000000000000000, 0.000000000000000000 ) ) ;
#8464 = EDGE_CURVE ( 'NONE', #20489, #11946, #1446, .T. ) ;
#8465 = CARTESIAN_POINT ( 'NONE',  ( 0.000000000000000000, 0.000000000000000000, -0.01377952755905511792 ) ) ;
#8466 = DIRECTION ( 'NONE',  ( 0.000000000000000000, 0.000000000000000000, -1.000000000000000000 ) ) ;
#8467 = FACE_OUTER_BOUND ( 'NONE', #4221, .T. ) ;
#8468 = DIRECTION ( 'NONE',  ( 0.000000000000000000, 0.000000000000000000, -1.000000000000000000 ) ) ;
#8469 = DIRECTION ( 'NONE',  ( 1.000000000000000000, 0.000000000000000000, 0.000000000000000000 ) ) ;
#8470 = FACE_OUTER_BOUND ( 'NONE', #19491, .T. ) ;
#8471 = B_SPLINE_CURVE_WITH_KNOTS ( 'NONE', 3,
 ( #6442, #6588, #4188, #19292, #15714, #601, #4824, #23691, #10534, #8291 ),
 .UNSPECIFIED., .F., .F.,
 ( 4, 2, 2, 2, 4 ),
 ( 0.000000000000000000, 0.1250000000000000000, 0.2500000000000000000, 0.3750000000000000000, 0.5000000000000000000 ),
 .UNSPECIFIED. ) ;
#8472 = CARTESIAN_POINT ( 'NONE',  ( -0.04838950581350995317, 0.1968503937007873850, -3.209671902477075900 ) ) ;
#8473 = VERTEX_POINT ( 'NONE', #10073 ) ;
#8474 = AXIS2_PLACEMENT_3D ( 'NONE', #3004, #9226, #9368 ) ;
#8475 = CARTESIAN_POINT ( 'NONE',  ( 0.3267210193396165585, -0.1884333032645078565, 0.07637549214372835182 ) ) ;
#8476 = ORIENTED_EDGE ( 'NONE', *, *, #1788, .T. ) ;
#8477 = ADVANCED_FACE ( 'NONE', ( #3716 ), #2772, .T. ) ;
#8478 = ORIENTED_EDGE ( 'NONE', *, *, #9199, .F. ) ;
#8479 = DIRECTION ( 'NONE',  ( -0.000000000000000000, -1.000000000000000000, -0.000000000000000000 ) ) ;
#8480 = CARTESIAN_POINT ( 'NONE',  ( 0.0007856387884314597293, 0.7354206117110280161, 0.2763636194372742216 ) ) ;
#8481 = CARTESIAN_POINT ( 'NONE',  ( 0.5476281405333178753, -0.07214854559198131956, 0.9202755905511811330 ) ) ;
#8482 = VERTEX_POINT ( 'NONE', #19112 ) ;
#8483 = CARTESIAN_POINT ( 'NONE',  ( -0.6562077975700374433, -2.731848031496062854E-17, -0.07874015748031495954 ) ) ;
#8484 = VERTEX_POINT ( 'NONE', #1460 ) ;
#8485 = EDGE_CURVE ( 'NONE', #6596, #22691, #15881, .T. ) ;
#8486 = CARTESIAN_POINT ( 'NONE',  ( 0.000000000000000000, 0.000000000000000000, 0.1992125984251968684 ) ) ;
#8487 = ( CONVERSION_BASED_UNIT ( 'INCH', #10883 ) LENGTH_UNIT ( ) NAMED_UNIT ( #22953 ) ) ;
#8488 = CARTESIAN_POINT ( 'NONE',  ( 0.000000000000000000, 0.000000000000000000, 0.03818897637795275884 ) ) ;
#8489 = DIRECTION ( 'NONE',  ( 0.000000000000000000, 0.000000000000000000, 1.000000000000000000 ) ) ;
#8490 = LINE ( 'NONE', #14338, #25043 ) ;
#8491 = EDGE_CURVE ( 'NONE', #21339, #19933, #6128, .T. ) ;
#8492 = CONICAL_SURFACE ( 'NONE', #18380, 0.4863540308881693086, 1.365720138124999927 ) ;
#8493 = AXIS2_PLACEMENT_3D ( 'NONE', #15298, #4540, #17529 ) ;
#8494 = ORIENTED_EDGE ( 'NONE', *, *, #13983, .T. ) ;
#8495 = CARTESIAN_POINT ( 'NONE',  ( 0.6709908451338799651, -0.1528902114222700781, 0.1322810039474933141 ) ) ;
#8496 = FACE_OUTER_BOUND ( 'NONE', #22266, .T. ) ;
#8497 = CARTESIAN_POINT ( 'NONE',  ( -0.2078289949484350141, -0.4330237525397957477, 0.2362204724409447676 ) ) ;
#8498 = CARTESIAN_POINT ( 'NONE',  ( 0.000000000000000000, 0.4724409448818898127, 0.000000000000000000 ) ) ;
#8499 = ( GEOMETRIC_REPRESENTATION_CONTEXT ( 3 ) GLOBAL_UNCERTAINTY_ASSIGNED_CONTEXT ( ( #20901 ) ) GLOBAL_UNIT_ASSIGNED_CONTEXT ( ( #1336, #3292, #20966 ) ) REPRESENTATION_CONTEXT ( 'NONE', 'WORKASPACE' ) ) ;
#8500 = CARTESIAN_POINT ( 'NONE',  ( 0.6241612306989096082, 0.1093779649447741559, 0.2481708550952254622 ) ) ;
#8501 = CARTESIAN_POINT ( 'NONE',  ( -0.5376957092749378164, -0.3112026930392873814, 0.2574803149606298969 ) ) ;
#8502 = CARTESIAN_POINT ( 'NONE',  ( 0.4954197419817713000, 0.2442565704126274662, 0.9399606299212598381 ) ) ;
#8503 = CARTESIAN_POINT ( 'NONE',  ( 0.1606879121748897576, -0.4409237942971110380, 0.07637549214372854611 ) ) ;
#8504 = ORIENTED_EDGE ( 'NONE', *, *, #10361, .F. ) ;
#8505 = CARTESIAN_POINT ( 'NONE',  ( 0.1151343661286149123, 0.3392608232659918288, -3.115157480314960647 ) ) ;
#8506 = EDGE_CURVE ( 'NONE', #14095, #7957, #15004, .T. ) ;
#8507 = EDGE_LOOP ( 'NONE', ( #20510, #14361, #9125, #2718 ) ) ;
#8508 = VERTEX_POINT ( 'NONE', #1601 ) ;
#8509 = CONICAL_SURFACE ( 'NONE', #17949, 0.4527559054764771496, 0.7853981642949022790 ) ;
#8510 = CARTESIAN_POINT ( 'NONE',  ( 0.2564944395535923571, -0.4441657790094409863, -1.550196850393700920 ) ) ;
#8511 = CARTESIAN_POINT ( 'NONE',  ( 0.5708647227724241713, -0.03746919241596944478, 0.9399606299212595051 ) ) ;
#8512 = DIRECTION ( 'NONE',  ( 0.000000000000000000, 0.7626852297620280163, 0.6467698511084468693 ) ) ;
#8513 = FACE_BOUND ( 'NONE', #2970, .T. ) ;
#8514 = CARTESIAN_POINT ( 'NONE',  ( 0.2662790972926426525, -0.4613045817969299023, 1.747047244094488416 ) ) ;
#8515 = EDGE_LOOP ( 'NONE', ( #592, #18928, #22938, #7216 ) ) ;
#8516 = EDGE_CURVE ( 'NONE', #16219, #14534, #8216, .T. ) ;
#8517 = CARTESIAN_POINT ( 'NONE',  ( 0.6711032387266614441, -0.1523958994813204848, 0.1322834645669291320 ) ) ;
#8518 = EDGE_CURVE ( 'NONE', #4351, #7455, #11155, .T. ) ;
#8519 = CIRCLE ( 'NONE', #10330, 0.1771653543307086798 ) ;
#8520 = AXIS2_PLACEMENT_3D ( 'NONE', #4717, #7251, #4989 ) ;
#8521 = DIRECTION ( 'NONE',  ( 0.2384530002628483802, 2.920207035189802662E-17, -0.9711540385879295911 ) ) ;
#8522 = DIRECTION ( 'NONE',  ( -0.6427876096865396960, -0.7660444431189776804, 0.000000000000000000 ) ) ;
#8523 = CARTESIAN_POINT ( 'NONE',  ( 0.000000000000000000, 0.000000000000000000, 0.6299212598425196763 ) ) ;
#8524 = EDGE_CURVE ( 'NONE', #2247, #3630, #19934, .T. ) ;
#8525 = ORIENTED_EDGE ( 'NONE', *, *, #6267, .T. ) ;
#8526 = PRESENTATION_STYLE_ASSIGNMENT (( #93 ) ) ;
#8527 = DIRECTION ( 'NONE',  ( 1.000000000000000000, 0.000000000000000000, 0.000000000000000000 ) ) ;
#8528 = ORIENTED_EDGE ( 'NONE', *, *, #20884, .F. ) ;
#8529 = EDGE_CURVE ( 'NONE', #13707, #12080, #15855, .T. ) ;
#8530 = AXIS2_PLACEMENT_3D ( 'NONE', #14081, #12521, #3466 ) ;
#8531 = PRODUCT_DEFINITION_CONTEXT ( 'detailed design', #14720, 'design' ) ;
#8532 = CARTESIAN_POINT ( 'NONE',  ( 0.4069519308877023178, -0.2006393256663573099, -1.934055118110236338 ) ) ;
#8533 = AXIS2_PLACEMENT_3D ( 'NONE', #11334, #10924, #23794 ) ;
#8534 = CIRCLE ( 'NONE', #26537, 0.06200787401574803237 ) ;
#8535 = APPLICATION_CONTEXT ( 'automotive_design' ) ;
#8536 = EDGE_CURVE ( 'NONE', #4501, #22748, #14225, .T. ) ;
#8537 = FACE_BOUND ( 'NONE', #24114, .T. ) ;
#8538 = ORIENTED_EDGE ( 'NONE', *, *, #18680, .T. ) ;
#8539 = CIRCLE ( 'NONE', #22532, 1.092519685039370136 ) ;
#8540 = CARTESIAN_POINT ( 'NONE',  ( -0.5546128944410685380, -0.2725325685736035286, -0.1175119830017629929 ) ) ;
#8541 = CARTESIAN_POINT ( 'NONE',  ( 0.000000000000000000, 0.09092130223458683158, -0.3779527559055118058 ) ) ;
#8542 = ITEM_DEFINED_TRANSFORMATION ( 'NONE', 'NONE', #14329,  #11588 ) ;
#8543 = DIRECTION ( 'NONE',  ( 1.000000000000000000, 0.000000000000000000, 0.000000000000000000 ) ) ;
#8544 = CARTESIAN_POINT ( 'NONE',  ( 0.000000000000000000, 0.000000000000000000, -1.550196850393700920 ) ) ;
#8545 = DIRECTION ( 'NONE',  ( -0.000000000000000000, -0.000000000000000000, -1.000000000000000000 ) ) ;
#8546 = CARTESIAN_POINT ( 'NONE',  ( -8.427884271297532088E-17, -0.6881889763779527325, 0.3401574803149606252 ) ) ;
#8547 = CARTESIAN_POINT ( 'NONE',  ( 0.1522836969735573143, 0.000000000000000000, 0.000000000000000000 ) ) ;
#8548 = CARTESIAN_POINT ( 'NONE',  ( -0.1970988029427959420, 0.3995913070737888706, -1.934055118110236338 ) ) ;
#8549 = EDGE_LOOP ( 'NONE', ( #8666, #1300, #15830, #1491, #6372, #15652 ) ) ;
#8550 = CARTESIAN_POINT ( 'NONE',  ( -0.1141709026133645999, 0.3362336590883638343, 1.953740157480315043 ) ) ;
#8551 = ORIENTED_EDGE ( 'NONE', *, *, #15454, .T. ) ;
#8552 = EDGE_CURVE ( 'NONE', #14474, #14467, #17557, .T. ) ;
#8553 = CARTESIAN_POINT ( 'NONE',  ( -0.5948382950512706158, -0.1382708294208072619, -0.2480148272232753359 ) ) ;
#8554 = CONICAL_SURFACE ( 'NONE', #27520, 0.6246466694403326469, 0.2617993874999998694 ) ;
#8555 = CARTESIAN_POINT ( 'NONE',  ( -0.5484420430267122892, -0.3174147232945255803, 0.2481708550949786873 ) ) ;
#8556 = CARTESIAN_POINT ( 'NONE',  ( 0.1532705055535415473, -0.5147072688414000563, -0.4165008336377047371 ) ) ;
#8557 = ORIENTED_EDGE ( 'NONE', *, *, #10907, .F. ) ;
#8558 = CARTESIAN_POINT ( 'NONE',  ( -2.685748425196850164E-17, 0.000000000000000000, -3.036417322828325105 ) ) ;
#8559 = EDGE_CURVE ( 'NONE', #24641, #17699, #2050, .T. ) ;
#8560 = ADVANCED_FACE ( 'NONE', ( #10919 ), #141, .T. ) ;
#8561 = CARTESIAN_POINT ( 'NONE',  ( -0.2272836761398000505, 0.2962590301041647667, -3.115157480314960647 ) ) ;
#8562 = DIRECTION ( 'NONE',  ( 0.8660254037844385966, 0.4999999999999998335, 0.000000000000000000 ) ) ;
#8563 = CARTESIAN_POINT ( 'NONE',  ( 0.3263749705684267921, -0.1890319631540330891, 0.1992125984251968684 ) ) ;
#8564 = LINE ( 'NONE', #10248, #16240 ) ;
#8565 = DIRECTION ( 'NONE',  ( 1.000000000000000000, 0.000000000000000000, 0.000000000000000000 ) ) ;
#8566 = B_SPLINE_CURVE_WITH_KNOTS ( 'NONE', 3,
 ( #20657, #16286, #5545, #16417, #18231, #7952 ),
 .UNSPECIFIED., .F., .F.,
 ( 4, 2, 4 ),
 ( 1.162880698919837918, 1.164573402063411978, 1.166266105206986037 ),
 .UNSPECIFIED. ) ;
#8567 = CIRCLE ( 'NONE', #6779, 0.4692913385826771866 ) ;
#8568 = ORIENTED_EDGE ( 'NONE', *, *, #23619, .T. ) ;
#8569 = CARTESIAN_POINT ( 'NONE',  ( -0.4790450267014849661, 0.08506312949783263744, 0.2467937632971976825 ) ) ;
#8570 = ORIENTED_EDGE ( 'NONE', *, *, #11608, .F. ) ;
#8571 = ORIENTED_EDGE ( 'NONE', *, *, #22943, .F. ) ;
#8572 = LINE ( 'NONE', #21570, #16465 ) ;
#8573 = CARTESIAN_POINT ( 'NONE',  ( -0.05118110236220472370, 0.000000000000000000, 0.000000000000000000 ) ) ;
#8574 = CARTESIAN_POINT ( 'NONE',  ( 0.7874015748031496509, -0.3839064563524838825, -0.3321176343386787466 ) ) ;
#8575 = FACE_OUTER_BOUND ( 'NONE', #1694, .T. ) ;
#8576 = CARTESIAN_POINT ( 'NONE',  ( -0.3382184156732166436, 0.3855916753051391033, 1.747047244094488194 ) ) ;
#8577 = DIRECTION ( 'NONE',  ( 1.000000000000000000, 7.017814999999989339E-18, 0.000000000000000000 ) ) ;
#8578 = VERTEX_POINT ( 'NONE', #13312 ) ;
#8580 = CARTESIAN_POINT ( 'NONE',  ( 0.3213305936751379432, -0.1584254766472190656, -3.115157480314960647 ) ) ;
#8579 = CARTESIAN_POINT ( 'NONE',  ( -0.6239291699170932404, 0.1106940470470682975, 0.2481708550940099900 ) ) ;
#8581 = ORIENTED_EDGE ( 'NONE', *, *, #13011, .T. ) ;
#8582 = ORIENTED_EDGE ( 'NONE', *, *, #9817, .F. ) ;
#8583 = CARTESIAN_POINT ( 'NONE',  ( -0.2817828961649163078, -0.3666644560843326794, -1.928289503579157405 ) ) ;
#8584 = ( LENGTH_UNIT ( ) NAMED_UNIT ( * ) SI_UNIT ( $, .METRE. ) ) ;
#8585 = CARTESIAN_POINT ( 'NONE',  ( 0.3339160553493882300, 1.214868409966151530, -0.6104964979807637748 ) ) ;
#8586 = CARTESIAN_POINT ( 'NONE',  ( 0.1677079028045344034, -0.2904160862623691997, 1.973425196850393970 ) ) ;
#8587 = VERTEX_POINT ( 'NONE', #10779 ) ;
#8588 = ORIENTED_EDGE ( 'NONE', *, *, #5907, .T. ) ;
#8589 = ORIENTED_EDGE ( 'NONE', *, *, #21703, .T. ) ;
#8590 = FACE_OUTER_BOUND ( 'NONE', #13893, .T. ) ;
#8591 = VERTEX_POINT ( 'NONE', #25620 ) ;
#8592 = VERTEX_POINT ( 'NONE', #11189 ) ;
#8593 = ORIENTED_EDGE ( 'NONE', *, *, #22305, .T. ) ;
#8594 = DIRECTION ( 'NONE',  ( 0.000000000000000000, 1.000000000000000000, 0.000000000000000000 ) ) ;
#8595 = CARTESIAN_POINT ( 'NONE',  ( -0.03532354024591775193, -0.6299212598425196763, 0.000000000000000000 ) ) ;
#8596 = DIRECTION ( 'NONE',  ( -0.7071067818211439482, 0.000000000000000000, -0.7071067805519510863 ) ) ;
#8597 = ORIENTED_EDGE ( 'NONE', *, *, #26056, .T. ) ;
#8598 = CARTESIAN_POINT ( 'NONE',  ( 0.1623262587483975672, -0.4476804331163366513, 0.2330651858608774607 ) ) ;
#8599 = VECTOR ( 'NONE', #16469, 39.37007874015748854 ) ;
#8600 = CARTESIAN_POINT ( 'NONE',  ( 0.000000000000000000, 0.000000000000000000, 0.02362204724409448786 ) ) ;
#8601 = CARTESIAN_POINT ( 'NONE',  ( -0.2131049448083992270, -0.5835666837866889667, 0.09685039370078740717 ) ) ;
#8602 = ( NAMED_UNIT ( * ) SI_UNIT ( $, .STERADIAN. ) SOLID_ANGLE_UNIT ( ) ) ;
#8603 = CARTESIAN_POINT ( 'NONE',  ( -0.4121342552748326060, -0.2031943647053980340, -1.928289503579156960 ) ) ;
#8604 = DIRECTION ( 'NONE',  ( -1.000000000000000000, 0.000000000000000000, 0.000000000000000000 ) ) ;
#8605 = DIRECTION ( 'NONE',  ( 0.000000000000000000, 0.000000000000000000, 1.000000000000000000 ) ) ;
#8606 = DIRECTION ( 'NONE',  ( 0.000000000000000000, 0.000000000000000000, -1.000000000000000000 ) ) ;
#8607 = EDGE_CURVE ( 'NONE', #14590, #26957, #3676, .T. ) ;
#8608 = EDGE_CURVE ( 'NONE', #21729, #15613, #24305, .T. ) ;
#8609 = CARTESIAN_POINT ( 'NONE',  ( 0.02576258753919729791, 0.1968503937007873850, -3.176774343053085481 ) ) ;
#8610 = ORIENTED_EDGE ( 'NONE', *, *, #13706, .F. ) ;
#8611 = PRODUCT_RELATED_PRODUCT_CATEGORY ( 'part', '', ( #25836 ) ) ;
#8612 = ORIENTED_EDGE ( 'NONE', *, *, #25937, .F. ) ;
#8613 = DIRECTION ( 'NONE',  ( 1.000000000000000000, 0.000000000000000000, 0.000000000000000000 ) ) ;
#8614 = EDGE_CURVE ( 'NONE', #10869, #17871, #6420, .T. ) ;
#8615 = ORIENTED_EDGE ( 'NONE', *, *, #26620, .F. ) ;
#8616 = B_SPLINE_CURVE_WITH_KNOTS ( 'NONE', 3,
 ( #6120, #14755, #14604, #21068, #5834, #12601, #3986, #23361 ),
 .UNSPECIFIED., .F., .F.,
 ( 4, 2, 2, 4 ),
 ( 5.336250286676794493E-07, 0.0004434172983717934590, 0.0008863009717149191629, 0.001772068318401170788 ),
 .UNSPECIFIED. ) ;
#8617 = CARTESIAN_POINT ( 'NONE',  ( -0.5905511811023621549, 1.087444635826771533, -0.1051828227901525498 ) ) ;
#8618 = EDGE_CURVE ( 'NONE', #12716, #6246, #7104, .T. ) ;
#8619 = ADVANCED_FACE ( 'NONE', ( #2431 ), #7771, .F. ) ;
#8620 = DIRECTION ( 'NONE',  ( 0.000000000000000000, 1.000000000000000000, 0.000000000000000000 ) ) ;
#8621 = ORIENTED_EDGE ( 'NONE', *, *, #22494, .F. ) ;
#8622 = CARTESIAN_POINT ( 'NONE',  ( -0.5511811023622048555, 0.03607471876259065596, 0.9399606299212598381 ) ) ;
#8623 = FACE_BOUND ( 'NONE', #14820, .T. ) ;
#8624 = ORIENTED_EDGE ( 'NONE', *, *, #20229, .F. ) ;
#8625 = CARTESIAN_POINT ( 'NONE',  ( -0.4338922498494567348, -0.2500511477696472085, 0.09684874903502814492 ) ) ;
#8626 = CARTESIAN_POINT ( 'NONE',  ( -0.09842519685039370636, 0.07874015748031495954, -0.04546065111729338803 ) ) ;
#8627 = FACE_OUTER_BOUND ( 'NONE', #10739, .T. ) ;
#8628 = DIRECTION ( 'NONE',  ( 1.000000000000000000, 0.000000000000000000, 0.000000000000000000 ) ) ;
#8629 = CARTESIAN_POINT ( 'NONE',  ( -0.09842519685039366473, 0.1968503937007873850, -3.548228346456693050 ) ) ;
#8630 = DIRECTION ( 'NONE',  ( 1.000000000000000000, 0.000000000000000000, 0.000000000000000000 ) ) ;
#8631 = CARTESIAN_POINT ( 'NONE',  ( -0.4055118110236220486, 0.9448818897637796255, 0.1771653543307086520 ) ) ;
#8632 = ( BOUNDED_CURVE ( )  B_SPLINE_CURVE ( 2, ( #15446, #23644, #21375 ),
 .UNSPECIFIED., .F., .T. ) 
 B_SPLINE_CURVE_WITH_KNOTS ( ( 3, 3 ),
 ( 0.000000000000000000, 0.5842180690389588982 ),
 .UNSPECIFIED. ) 
 CURVE ( )  GEOMETRIC_REPRESENTATION_ITEM ( )  RATIONAL_B_SPLINE_CURVE ( ( 1.000000000000000000, 1.154700538379251906, 1.000000000000000000 ) ) 
 REPRESENTATION_ITEM ( '' )  ) ;
#8633 = CARTESIAN_POINT ( 'NONE',  ( -0.1771653543307086520, 0.1673228346456692994, 0.000000000000000000 ) ) ;
#8634 = TOROIDAL_SURFACE ( 'NONE', #6844, 0.4325730547867440712, 0.01377952755905511792 ) ;
#8635 = ( GEOMETRIC_REPRESENTATION_CONTEXT ( 3 ) GLOBAL_UNCERTAINTY_ASSIGNED_CONTEXT ( ( #20622 ) ) GLOBAL_UNIT_ASSIGNED_CONTEXT ( ( #10223, #14502, #18839 ) ) REPRESENTATION_CONTEXT ( 'NONE', 'WORKASPACE' ) ) ;
#8636 = DIRECTION ( 'NONE',  ( 0.000000000000000000, 0.000000000000000000, 1.000000000000000000 ) ) ;
#8637 = CARTESIAN_POINT ( 'NONE',  ( 0.06690297524255699180, -0.5085287184740814315, -1.550196850393700920 ) ) ;
#8638 = CIRCLE ( 'NONE', #6392, 0.3543307086367249448 ) ;
#8639 = CYLINDRICAL_SURFACE ( 'NONE', #26341, 0.4807043897637795493 ) ;
#8640 = ORIENTED_EDGE ( 'NONE', *, *, #4968, .T. ) ;
#8641 = DIRECTION ( 'NONE',  ( 0.000000000000000000, -1.000000000000000000, 0.000000000000000000 ) ) ;
#8642 = ORIENTED_EDGE ( 'NONE', *, *, #11446, .T. ) ;
#8643 = EDGE_CURVE ( 'NONE', #23407, #7809, #11363, .T. ) ;
#8644 = EDGE_CURVE ( 'NONE', #15443, #15651, #1893, .T. ) ;
#8645 = ORIENTED_EDGE ( 'NONE', *, *, #4507, .F. ) ;
#8646 = AXIS2_PLACEMENT_3D ( 'NONE', #4993, #13616, #22235 ) ;
#8647 = CARTESIAN_POINT ( 'NONE',  ( 0.5118110236220473341, -0.03349795313024152288, -1.550196850393700920 ) ) ;
#8648 = CARTESIAN_POINT ( 'NONE',  ( -0.3483099419450385037, -0.4538399017590776796, 0.9399606299212598381 ) ) ;
#8649 = ADVANCED_FACE ( 'NONE', ( #6548 ), #12040, .F. ) ;
#8650 = CARTESIAN_POINT ( 'NONE',  ( 0.000000000000000000, -5.457511811023621697E-17, -0.1696422624804970747 ) ) ;
#8651 = CARTESIAN_POINT ( 'NONE',  ( -0.2362204724225640262, 2.892866454453686688E-17, -4.291338582656260670 ) ) ;
#8652 = ORIENTED_EDGE ( 'NONE', *, *, #9739, .F. ) ;
#8653 = CARTESIAN_POINT ( 'NONE',  ( 0.5949363243629232079, -0.1357903337134992172, 0.2362204724409449064 ) ) ;
#8654 = VECTOR ( 'NONE', #3675, 39.37007874015748143 ) ;
#8655 = PRESENTATION_STYLE_ASSIGNMENT (( #222 ) ) ;
#8656 = DIRECTION ( 'NONE',  ( 1.000000000000000000, 0.000000000000000000, 0.000000000000000000 ) ) ;
#8657 = DIRECTION ( 'NONE',  ( -0.9790454724845842893, 0.1018208755700880375, -0.1763589297585410332 ) ) ;
#8658 = DIRECTION ( 'NONE',  ( -0.1736481776669313026, -0.9848077530122080203, 0.000000000000000000 ) ) ;
#8659 = CYLINDRICAL_SURFACE ( 'NONE', #22247, 1.377952755905512472 ) ;
#8660 = CARTESIAN_POINT ( 'NONE',  ( 0.1707210962531913734, -0.4707890492249701131, 0.09685039370078740717 ) ) ;
#8661 = ORIENTED_EDGE ( 'NONE', *, *, #13195, .F. ) ;
#8662 = ORIENTED_EDGE ( 'NONE', *, *, #22533, .F. ) ;
#8663 = DIRECTION ( 'NONE',  ( 1.000000000000000000, 0.000000000000000000, 0.000000000000000000 ) ) ;
#8664 = FACE_OUTER_BOUND ( 'NONE', #8515, .T. ) ;
#8665 = CARTESIAN_POINT ( 'NONE',  ( -0.2466292688015410683, 0.4270824798167730529, -1.550196850393700920 ) ) ;
#8666 = ORIENTED_EDGE ( 'NONE', *, *, #22284, .F. ) ;
#8667 = DIRECTION ( 'NONE',  ( 1.000000000000000000, 0.000000000000000000, 0.000000000000000000 ) ) ;
#8668 = CARTESIAN_POINT ( 'NONE',  ( 0.3929158813954871654, 0.2268989272875732710, -1.934055118110236338 ) ) ;
#8669 = AXIS2_PLACEMENT_3D ( 'NONE', #7795, #10318, #10172 ) ;
#8670 = ADVANCED_BREP_SHAPE_REPRESENTATION ( 'Deep Groove Ball Bearing 20x37x9', ( #22049, #11588 ), #25599 ) ;
#8671 = CARTESIAN_POINT ( 'NONE',  ( -0.5604501195268866143, 0.4479362078580881312, 0.3122824329294420775 ) ) ;
#8672 = EDGE_CURVE ( 'NONE', #8578, #2204, #18903, .T. ) ;
#8673 = AXIS2_PLACEMENT_3D ( 'NONE', #21001, #27087, #852 ) ;
#8674 = CARTESIAN_POINT ( 'NONE',  ( -0.6562077975700453258, 2.293650393700787223E-14, 0.07874015748031495954 ) ) ;
#8675 = DIRECTION ( 'NONE',  ( 0.000000000000000000, 0.000000000000000000, 1.000000000000000000 ) ) ;
#8676 = EDGE_CURVE ( 'NONE', #12052, #11811, #23099, .T. ) ;
#8677 = B_SPLINE_CURVE_WITH_KNOTS ( 'NONE', 3,
 ( #8145, #25365, #1913, #25511 ),
 .UNSPECIFIED., .F., .F.,
 ( 4, 4 ),
 ( 0.7172350147555668354, 0.7187013008684189908 ),
 .UNSPECIFIED. ) ;
#8678 = DIRECTION ( 'NONE',  ( -1.000000000000000000, 0.000000000000000000, 0.000000000000000000 ) ) ;
#8679 = DIRECTION ( 'NONE',  ( 0.000000000000000000, 0.000000000000000000, -1.000000000000000000 ) ) ;
#8680 = LINE ( 'NONE', #19420, #2520 ) ;
#8681 = PRODUCT_DEFINITION_SHAPE ( 'NONE', 'NONE',  #17410 ) ;
#8682 = CARTESIAN_POINT ( 'NONE',  ( -0.3018020646414484309, 0.3593743330771480560, 0.1992150590373740204 ) ) ;
#8683 = ADVANCED_FACE ( 'NONE', ( #25302 ), #23055, .T. ) ;
#8684 = ORIENTED_EDGE ( 'NONE', *, *, #22885, .T. ) ;
#8685 = AXIS2_PLACEMENT_3D ( 'NONE', #24793, #9960, #20569 ) ;
#8686 = CARTESIAN_POINT ( 'NONE',  ( -0.7635713814939685262, 0.3473852540523503785, 0.02512505594370720644 ) ) ;
#8687 = VERTEX_POINT ( 'NONE', #18938 ) ;
#8688 = VECTOR ( 'NONE', #2672, 39.37007874015748854 ) ;
#8689 = CARTESIAN_POINT ( 'NONE',  ( 0.2421724791772047192, 0.2891474103999575052, 0.07637630750536809898 ) ) ;
#8690 = LINE ( 'NONE', #15618, #18327 ) ;
#8691 = CARTESIAN_POINT ( 'NONE',  ( -0.4216473064036311280, -0.2427620699869365573, 0.1075369453531297426 ) ) ;
#8692 = CARTESIAN_POINT ( 'NONE',  ( 0.3102399269716953345, -1.013856135328759844, -0.5158482079756747662 ) ) ;
#8693 = DIRECTION ( 'NONE',  ( 0.000000000000000000, 1.000000000000000000, 0.000000000000000000 ) ) ;
#8694 = EDGE_CURVE ( 'NONE', #20821, #5717, #23639, .T. ) ;
#8695 = DIRECTION ( 'NONE',  ( 1.000000000000000000, 0.000000000000000000, 0.000000000000000000 ) ) ;
#8696 = DIRECTION ( 'NONE',  ( 0.000000000000000000, 0.000000000000000000, 1.000000000000000000 ) ) ;
#8697 = FACE_OUTER_BOUND ( 'NONE', #20863, .T. ) ;
#8698 = DIRECTION ( 'NONE',  ( 0.000000000000000000, -1.000000000000000000, 0.000000000000000000 ) ) ;
#8699 = ORIENTED_EDGE ( 'NONE', *, *, #5118, .F. ) ;
#8700 = CARTESIAN_POINT ( 'NONE',  ( 0.03937007874015747977, 0.000000000000000000, 0.000000000000000000 ) ) ;
#8701 = AXIS2_PLACEMENT_3D ( 'NONE', #3175, #1088, #20709 ) ;
#8702 = VERTEX_POINT ( 'NONE', #16404 ) ;
#8703 = CARTESIAN_POINT ( 'NONE',  ( 1.692913385826771533, 0.07874015748031495954, 3.109831496062992451E-16 ) ) ;
#8704 = VECTOR ( 'NONE', #21550, 39.37007874015748143 ) ;
#8705 = ORIENTED_EDGE ( 'NONE', *, *, #1983, .F. ) ;
#8706 = ORIENTED_EDGE ( 'NONE', *, *, #3861, .T. ) ;
#8707 = FACE_OUTER_BOUND ( 'NONE', #27744, .T. ) ;
#8708 = CARTESIAN_POINT ( 'NONE',  ( 0.3145317858139327627, 0.4092783051644230397, 1.766732283464566899 ) ) ;
#8709 = SHAPE_DEFINITION_REPRESENTATION ( #5976, #25798 ) ;
#8710 = CARTESIAN_POINT ( 'NONE',  ( 0.1327036767659630079, 0.4954415918530855056, 1.766732283464566899 ) ) ;
#8711 = EDGE_CURVE ( 'NONE', #12716, #20920, #5043, .T. ) ;
#8712 = CYLINDRICAL_SURFACE ( 'NONE', #19015, 0.3771653543307086909 ) ;
#8713 = VERTEX_POINT ( 'NONE', #12591 ) ;
#8714 = AXIS2_PLACEMENT_3D ( 'NONE', #15823, #5653, #14277 ) ;
#8715 = VERTEX_POINT ( 'NONE', #20926 ) ;
#8716 = CARTESIAN_POINT ( 'NONE',  ( 0.3574975638436101444, 0.02339816079119100625, -3.115157480314960647 ) ) ;
#8717 = EDGE_LOOP ( 'NONE', ( #12154, #5022, #11792, #2169 ) ) ;
#8718 = ORIENTED_EDGE ( 'NONE', *, *, #15227, .F. ) ;
#8719 = CYLINDRICAL_SURFACE ( 'NONE', #25858, 0.1181102362204724532 ) ;
#8720 = ( CONVERSION_BASED_UNIT ( 'INCH', #3134 ) LENGTH_UNIT ( ) NAMED_UNIT ( #24789 ) ) ;
#8721 = FACE_BOUND ( 'NONE', #16644, .T. ) ;
#8722 = CARTESIAN_POINT ( 'NONE',  ( 0.3007905576423883232, 0.1482986320106616795, 1.953740157480315043 ) ) ;
#8723 = VERTEX_POINT ( 'NONE', #25013 ) ;
#8724 = ORIENTED_EDGE ( 'NONE', *, *, #22982, .F. ) ;
#8725 = EDGE_CURVE ( 'NONE', #11982, #7640, #12720, .T. ) ;
#8726 = FACE_OUTER_BOUND ( 'NONE', #8147, .T. ) ;
#8727 = ORIENTED_EDGE ( 'NONE', *, *, #22521, .T. ) ;
#8728 = ORIENTED_EDGE ( 'NONE', *, *, #3742, .F. ) ;
#8729 = VERTEX_POINT ( 'NONE', #27008 ) ;
#8730 = DIRECTION ( 'NONE',  ( 0.000000000000000000, 0.000000000000000000, -1.000000000000000000 ) ) ;
#8731 = TOROIDAL_SURFACE ( 'NONE', #12330, 0.5393700787401575214, 0.01181102362204724393 ) ;
#8732 = VECTOR ( 'NONE', #11467, 39.37007874015748143 ) ;
#8733 = DIRECTION ( 'NONE',  ( 3.508907999999999048E-18, -0.4999999999999998890, 0.8660254037844388186 ) ) ;
#8734 = DIRECTION ( 'NONE',  ( 0.000000000000000000, 1.000000000000000000, 0.000000000000000000 ) ) ;
#8735 = CARTESIAN_POINT ( 'NONE',  ( 0.7772278266253901391, 0.5213247747914033781, 0.1262149107176392671 ) ) ;
#8736 = VECTOR ( 'NONE', #13821, 39.37007874015748143 ) ;
#8737 = AXIS2_PLACEMENT_3D ( 'NONE', #5042, #22143, #22279 ) ;
#8738 = DIRECTION ( 'NONE',  ( -0.000000000000000000, -1.000000000000000000, -0.000000000000000000 ) ) ;
#8739 = ITEM_DEFINED_TRANSFORMATION ( 'NONE', 'NONE', #4844,  #11588 ) ;
#8740 = AXIS2_PLACEMENT_3D ( 'NONE', #7910, #20761, #14274 ) ;
#8741 = CARTESIAN_POINT ( 'NONE',  ( 0.0006615832605804723319, 0.6212594902576319411, 0.2574803149606298969 ) ) ;
#8742 = DIRECTION ( 'NONE',  ( 1.000000000000000000, 0.000000000000000000, 0.000000000000000000 ) ) ;
#8743 = AXIS2_PLACEMENT_3D ( 'NONE', #7574, #11958, #20577 ) ;
#8744 = CARTESIAN_POINT ( 'NONE',  ( -0.3700489919980719522, -1.073999312313020926, -0.3399043508710541950 ) ) ;
#8745 = CARTESIAN_POINT ( 'NONE',  ( -0.5187889641967551313, -0.1190953285357212593, 0.1322834645669291320 ) ) ;
#8746 = DIRECTION ( 'NONE',  ( 0.000000000000000000, 0.000000000000000000, -1.000000000000000000 ) ) ;
#8747 = ADVANCED_FACE ( 'NONE', ( #12453 ), #7652, .F. ) ;
#8748 = AXIS2_PLACEMENT_3D ( 'NONE', #2953, #11584, #13700 ) ;
#8749 = CARTESIAN_POINT ( 'NONE',  ( 0.07874015748031489015, 0.1968503937007873850, -3.272637795275590733 ) ) ;
#8750 = ORIENTED_EDGE ( 'NONE', *, *, #7458, .T. ) ;
#8751 = ORIENTED_EDGE ( 'NONE', *, *, #2545, .F. ) ;
#8752 = FACE_OUTER_BOUND ( 'NONE', #21072, .T. ) ;
#8753 = ORIENTED_EDGE ( 'NONE', *, *, #7834, .F. ) ;
#8754 = VECTOR ( 'NONE', #25803, 39.37007874015748143 ) ;
#8755 = DIRECTION ( 'NONE',  ( 0.000000000000000000, 0.000000000000000000, 1.000000000000000000 ) ) ;
#8756 = CARTESIAN_POINT ( 'NONE',  ( -0.5714859364026961819, 1.109681230469752089, -0.06506513713611936089 ) ) ;
#8757 = DIRECTION ( 'NONE',  ( -1.000000000000000000, 0.000000000000000000, 0.000000000000000000 ) ) ;
#8758 = EDGE_LOOP ( 'NONE', ( #8312, #7015 ) ) ;
#8759 = CARTESIAN_POINT ( 'NONE',  ( 0.1429116519061227053, -0.5335524835332334792, 0.9202755905511811330 ) ) ;
#8760 = CARTESIAN_POINT ( 'NONE',  ( 5.827097576719993621E-17, 0.6881889763779529545, 0.3401599409343964431 ) ) ;
#8761 = ORIENTED_EDGE ( 'NONE', *, *, #5290, .T. ) ;
#8762 = CARTESIAN_POINT ( 'NONE',  ( 0.5511811023622047445, 0.000000000000000000, 0.2637795275590551491 ) ) ;
#8763 = DIRECTION ( 'NONE',  ( 0.000000000000000000, -1.000000000000000000, 0.000000000000000000 ) ) ;
#8764 = DIRECTION ( 'NONE',  ( 0.000000000000000000, 0.000000000000000000, -1.000000000000000000 ) ) ;
#8765 = FACE_OUTER_BOUND ( 'NONE', #17023, .T. ) ;
#8766 = AXIS2_PLACEMENT_3D ( 'NONE', #8197, #21335, #10578 ) ;
#8767 = CARTESIAN_POINT ( 'NONE',  ( -0.1718374205099799101, -0.4703827404237102550, 0.09685039370078740717 ) ) ;
#8768 = DIRECTION ( 'NONE',  ( 0.4999999999999994449, -0.8660254037844389297, 0.000000000000000000 ) ) ;
#8769 = CARTESIAN_POINT ( 'NONE',  ( 0.000000000000000000, 0.000000000000000000, 0.07637795275590551769 ) ) ;
#8770 = DIRECTION ( 'NONE',  ( 0.000000000000000000, 7.180547322999999937E-06, -0.9999999999742198442 ) ) ;
#8771 = CARTESIAN_POINT ( 'NONE',  ( -0.3334645669291338987, 9.254566433503937147E-06, -2.341456692880161228 ) ) ;
#8772 = CARTESIAN_POINT ( 'NONE',  ( -0.3482225189666627863, 0.4539000224941008854, 0.9399606299212598381 ) ) ;
#8773 = ADVANCED_FACE ( 'NONE', ( #20644 ), #3830, .T. ) ;
#8774 = AXIS2_PLACEMENT_3D ( 'NONE', #27452, #14623, #18961 ) ;
#8775 = CARTESIAN_POINT ( 'NONE',  ( 0.4130706566799093316, 0.6693539628600351232, 1.355058665357500095E-17 ) ) ;
#8776 = EDGE_LOOP ( 'NONE', ( #17052, #12323, #26672, #8433 ) ) ;
#8777 = DIRECTION ( 'NONE',  ( -0.9659258263664933786, -0.2588190448135666011, 0.000000000000000000 ) ) ;
#8778 = ORIENTED_EDGE ( 'NONE', *, *, #15964, .T. ) ;
#8779 = ORIENTED_EDGE ( 'NONE', *, *, #25516, .T. ) ;
#8780 = CIRCLE ( 'NONE', #257, 0.6881889763779527325 ) ;
#8781 = ORIENTED_EDGE ( 'NONE', *, *, #14920, .F. ) ;
#8782 = CARTESIAN_POINT ( 'NONE',  ( -0.2860025288253731923, -0.4954757973265057069, 0.9399606299212601712 ) ) ;
#8783 = DIRECTION ( 'NONE',  ( 0.000000000000000000, 0.000000000000000000, 1.000000000000000000 ) ) ;
#8784 = LINE ( 'NONE', #15318, #23662 ) ;
#8785 = CARTESIAN_POINT ( 'NONE',  ( -0.2230788859036006710, 0.2650812153444457864, 0.1478915661164160456 ) ) ;
#8786 = ORIENTED_EDGE ( 'NONE', *, *, #11893, .F. ) ;
#8787 = ORIENTED_EDGE ( 'NONE', *, *, #6802, .T. ) ;
#8788 = CIRCLE ( 'NONE', #10602, 0.2395669291338582696 ) ;
#8789 = CARTESIAN_POINT ( 'NONE',  ( 0.003937007874015826907, 0.09842519685039370636, 0.000000000000000000 ) ) ;
#8790 = CIRCLE ( 'NONE', #16916, 0.3031496062992122820 ) ;
#8791 = FACE_OUTER_BOUND ( 'NONE', #7642, .T. ) ;
#8792 = DIRECTION ( 'NONE',  ( 0.7660444431189777914, -0.6427876096865395850, 0.000000000000000000 ) ) ;
#8793 = CARTESIAN_POINT ( 'NONE',  ( -0.4334967711386992772, -0.2507361369899905879, 0.2574819596263889787 ) ) ;
#8794 = EDGE_CURVE ( 'NONE', #5423, #10634, #15444, .T. ) ;
#8795 = DIRECTION ( 'NONE',  ( 0.000000000000000000, 0.000000000000000000, 1.000000000000000000 ) ) ;
#8796 = DIRECTION ( 'NONE',  ( 0.000000000000000000, 0.000000000000000000, 1.000000000000000000 ) ) ;
#8797 = EDGE_CURVE ( 'NONE', #15630, #25955, #27615, .T. ) ;
#8798 = EDGE_LOOP ( 'NONE', ( #228, #18031, #2852, #21172, #8172, #732 ) ) ;
#8799 = LINE ( 'NONE', #476, #17546 ) ;
#8800 = LINE ( 'NONE', #26305, #23461 ) ;
#8801 = CARTESIAN_POINT ( 'NONE',  ( -0.4763861460130343062, -0.1275996891957688339, -1.569881889763779625 ) ) ;
#8802 = EDGE_CURVE ( 'NONE', #27102, #4182, #10018, .T. ) ;
#8803 = AXIS2_PLACEMENT_3D ( 'NONE', #24673, #18591, #18308 ) ;
#8804 = CARTESIAN_POINT ( 'NONE',  ( -0.4585215200179055817, -0.03001016326912892690, -1.928289503579156516 ) ) ;
#8805 = B_SPLINE_CURVE_WITH_KNOTS ( 'NONE', 3,
 ( #7975, #12792, #6580, #17448 ),
 .UNSPECIFIED., .F., .F.,
 ( 4, 4 ),
 ( 1.743059029969430185, 1.744705333033729877 ),
 .UNSPECIFIED. ) ;
#8806 = EDGE_CURVE ( 'NONE', #22294, #12664, #26679, .T. ) ;
#8807 = DIRECTION ( 'NONE',  ( 0.000000000000000000, 1.000000000000000000, 0.000000000000000000 ) ) ;
#8808 = CARTESIAN_POINT ( 'NONE',  ( -0.5781866216478808163, 0.4620966632763692794, 0.2161412452687943575 ) ) ;
#8809 = AXIS2_PLACEMENT_3D ( 'NONE', #6139, #7964, #20808 ) ;
#8810 = ORIENTED_EDGE ( 'NONE', *, *, #6051, .F. ) ;
#8811 = AXIS2_PLACEMENT_3D ( 'NONE', #27856, #4257, #18544 ) ;
#8812 = CARTESIAN_POINT ( 'NONE',  ( -0.6505662911506299162, -0.01547120374406815019, -0.07881933527123072269 ) ) ;
#8813 = ( NAMED_UNIT ( * ) SI_UNIT ( $, .STERADIAN. ) SOLID_ANGLE_UNIT ( ) ) ;
#8814 = DIRECTION ( 'NONE',  ( 1.000000000000000000, 0.000000000000000000, 0.000000000000000000 ) ) ;
#8815 = ORIENTED_EDGE ( 'NONE', *, *, #19826, .F. ) ;
#8816 = CARTESIAN_POINT ( 'NONE',  ( 0.000000000000000000, 0.000000000000000000, 0.03818897637795275884 ) ) ;
#8817 = ORIENTED_EDGE ( 'NONE', *, *, #3861, .F. ) ;
#8818 = FACE_OUTER_BOUND ( 'NONE', #17481, .T. ) ;
#8819 = AXIS2_PLACEMENT_3D ( 'NONE', #13261, #6914, #4634 ) ;
#8820 = ORIENTED_EDGE ( 'NONE', *, *, #5893, .F. ) ;
#8821 = CARTESIAN_POINT ( 'NONE',  ( -0.7795729917428700917, 0.4543402377591519992, 0.1538738033641767755 ) ) ;
#8822 = ORIENTED_EDGE ( 'NONE', *, *, #23952, .T. ) ;
#8823 = CARTESIAN_POINT ( 'NONE',  ( 0.003937007874015826907, -4.393043307086613241E-18, -0.1023622047244094474 ) ) ;
#8824 = DIRECTION ( 'NONE',  ( 0.000000000000000000, 0.9850313626640179177, -0.1723752144836030176 ) ) ;
#8825 = CARTESIAN_POINT ( 'NONE',  ( 0.3334645669291338987, -1.269546425348450747, -0.8304542831125020230 ) ) ;
#8826 = ORIENTED_EDGE ( 'NONE', *, *, #1471, .T. ) ;
#8827 = CARTESIAN_POINT ( 'NONE',  ( 1.687505431895960050E-16, 0.07874015748031495954, 1.377952755905512472 ) ) ;
#8828 = CARTESIAN_POINT ( 'NONE',  ( -0.09842519685039370636, -0.07874015748031495954, 0.04546065111729331171 ) ) ;
#8829 = CARTESIAN_POINT ( 'NONE',  ( -0.3233561589688984661, 0.1867299569291787087, -3.115157480314960647 ) ) ;
#8830 = AXIS2_PLACEMENT_3D ( 'NONE', #15168, #26025, #2153 ) ;
#8831 = LINE ( 'NONE', #19293, #5294 ) ;
#8832 = PLANE ( 'NONE',  #1124 ) ;
#8833 = FACE_OUTER_BOUND ( 'NONE', #4863, .T. ) ;
#8834 = EDGE_CURVE ( 'NONE', #11924, #6276, #27573, .T. ) ;
#8835 = ORIENTED_EDGE ( 'NONE', *, *, #24370, .T. ) ;
#8836 = CARTESIAN_POINT ( 'NONE',  ( 0.000000000000000000, 0.000000000000000000, -3.278217716535432842E-17 ) ) ;
#8837 = CIRCLE ( 'NONE', #7485, 0.02362204724409448092 ) ;
#8838 = VERTEX_POINT ( 'NONE', #18646 ) ;
#8839 = ORIENTED_EDGE ( 'NONE', *, *, #2085, .F. ) ;
#8840 = CARTESIAN_POINT ( 'NONE',  ( 0.4084310843292833226, 0.3265597623332965882, 0.3331434174623317257 ) ) ;
#8841 = DIRECTION ( 'NONE',  ( 1.000000000000000000, 0.000000000000000000, 0.000000000000000000 ) ) ;
#8842 = PRODUCT_CONTEXT ( 'NONE', #19006, 'mechanical' ) ;
#8843 = CARTESIAN_POINT ( 'NONE',  ( -0.06699507805369007973, 0.5085118447801436625, 1.766732283464566899 ) ) ;
#8844 = ORIENTED_EDGE ( 'NONE', *, *, #2388, .F. ) ;
#8845 = CYLINDRICAL_SURFACE ( 'NONE', #21731, 0.6889763779527560139 ) ;
#8846 = VERTEX_POINT ( 'NONE', #27284 ) ;
#8847 = EDGE_LOOP ( 'NONE', ( #11177, #19226, #26433, #1079 ) ) ;
#8849 = CARTESIAN_POINT ( 'NONE',  ( 0.1200583359873108324, 0.3535721684717922364, -3.115157480314960647 ) ) ;
#8848 = FACE_OUTER_BOUND ( 'NONE', #8758, .T. ) ;
#8850 = AXIS2_PLACEMENT_3D ( 'NONE', #17642, #22161, #24006 ) ;
#8851 = VERTEX_POINT ( 'NONE', #6514 ) ;
#8852 = ( NAMED_UNIT ( * ) PLANE_ANGLE_UNIT ( ) SI_UNIT ( $, .RADIAN. ) ) ;
#8853 = CARTESIAN_POINT ( 'NONE',  ( 0.4684132450478840637, -0.1062614382955253817, 0.2194422276453884824 ) ) ;
#8854 = CARTESIAN_POINT ( 'NONE',  ( 0.2660793235464212203, 0.2041304421298323901, 1.953740157480315043 ) ) ;
#8855 = ORIENTED_EDGE ( 'NONE', *, *, #8116, .F. ) ;
#8856 = AXIS2_PLACEMENT_3D ( 'NONE', #8650, #2284, #8919 ) ;
#8857 = CARTESIAN_POINT ( 'NONE',  ( 0.6117448998508543401, 0.1083144418130956715, 0.09684874924366436433 ) ) ;
#8858 = ORIENTED_EDGE ( 'NONE', *, *, #4888, .F. ) ;
#8859 = VERTEX_POINT ( 'NONE', #4393 ) ;
#8860 = VERTEX_POINT ( 'NONE', #21769 ) ;
#8861 = DIRECTION ( 'NONE',  ( 0.000000000000000000, 1.000000000000000000, 0.000000000000000000 ) ) ;
#8862 = EDGE_CURVE ( 'NONE', #21888, #19645, #4659, .T. ) ;
#8863 = CONTEXT_DEPENDENT_SHAPE_REPRESENTATION ( #780, #13422 ) ;
#8864 = EDGE_CURVE ( 'NONE', #11261, #20886, #1853, .T. ) ;
#8865 = CARTESIAN_POINT ( 'NONE',  ( 0.3976891862754212137, 1.133679329692560911, -0.4395307839725701160 ) ) ;
#8866 = CARTESIAN_POINT ( 'NONE',  ( 0.6936167303942817330, 0.7750952645509693317, -0.02289373067002851980 ) ) ;
#8867 = VERTEX_POINT ( 'NONE', #17385 ) ;
#8868 = EDGE_CURVE ( 'NONE', #16539, #22124, #11026, .T. ) ;
#8869 = AXIS2_PLACEMENT_3D ( 'NONE', #10438, #14850, #10575 ) ;
#8870 = B_SPLINE_CURVE_WITH_KNOTS ( 'NONE', 3,
 ( #15452, #22061, #350, #23923, #19944, #24046, #21522, #598, #8929, #9191 ),
 .UNSPECIFIED., .F., .F.,
 ( 4, 2, 2, 2, 4 ),
 ( 0.000000000000000000, 0.2500000000000001110, 0.5000000000000002220, 0.7500000000000003331, 1.000000000000000000 ),
 .UNSPECIFIED. ) ;
#8871 = CARTESIAN_POINT ( 'NONE',  ( 0.3174445073404819628, -0.1826860508837442609, 0.1910323753066165142 ) ) ;
#8872 = VECTOR ( 'NONE', #1329, 39.37007874015748143 ) ;
#8873 = DIRECTION ( 'NONE',  ( -1.000000000000000000, 0.000000000000000000, 0.000000000000000000 ) ) ;
#8874 = AXIS2_PLACEMENT_3D ( 'NONE', #19907, #13127, #22027 ) ;
#8875 = CARTESIAN_POINT ( 'NONE',  ( -0.3724354128627712091, -1.063775794758070603, -0.3247274185435837235 ) ) ;
#8876 = EDGE_LOOP ( 'NONE', ( #2228, #23043, #11268, #23391, #4453 ) ) ;
#8877 = DIRECTION ( 'NONE',  ( 1.000000000000000000, 0.000000000000000000, 0.000000000000000000 ) ) ;
#8878 = DIRECTION ( 'NONE',  ( 0.000000000000000000, 0.000000000000000000, 1.000000000000000000 ) ) ;
#8879 = CARTESIAN_POINT ( 'NONE',  ( -0.0005789221761214173069, 0.4692909815006417462, 0.07637795275590551769 ) ) ;
#8880 = EDGE_CURVE ( 'NONE', #19062, #17310, #13156, .T. ) ;
#8881 = CARTESIAN_POINT ( 'NONE',  ( -0.01288382760289588994, 0.2165354330708661457, -3.174212598425197207 ) ) ;
#8882 = ORIENTED_EDGE ( 'NONE', *, *, #868, .T. ) ;
#8883 = DIRECTION ( 'NONE',  ( -0.000000000000000000, 1.000000000000000000, -0.000000000000000000 ) ) ;
#8884 = CARTESIAN_POINT ( 'NONE',  ( 0.3184623230426910645, -0.1570784101598338978, 1.953740157480315043 ) ) ;
#8885 = EDGE_LOOP ( 'NONE', ( #15087, #20355, #8844, #5825 ) ) ;
#8886 = CARTESIAN_POINT ( 'NONE',  ( -0.4062254136079394562, -0.2349793847444822670, 0.07637630773773071424 ) ) ;
#8887 = VERTEX_POINT ( 'NONE', #4118 ) ;
#8888 = DIRECTION ( 'NONE',  ( 1.000000000000000000, 0.000000000000000000, 0.000000000000000000 ) ) ;
#8889 = CARTESIAN_POINT ( 'NONE',  ( 0.1522836969735572310, -0.4941010236220472751, 6.050992370341708321E-17 ) ) ;
#8890 = AXIS2_PLACEMENT_3D ( 'NONE', #18878, #26691, #1658 ) ;
#8891 = CARTESIAN_POINT ( 'NONE',  ( 0.7871730179869745880, 0.4038169352867496120, 0.1713250154738354125 ) ) ;
#8892 = B_SPLINE_CURVE_WITH_KNOTS ( 'NONE', 3,
 ( #16823, #14732, #14995, #20662, #12847, #16292, #2118, #1974, #10736, #12579 ),
 .UNSPECIFIED., .F., .F.,
 ( 4, 2, 2, 2, 4 ),
 ( 0.000000000000000000, 0.2499999999999998890, 0.4999999999999997780, 0.7499999999999996669, 1.000000000000000000 ),
 .UNSPECIFIED. ) ;
#8893 = ORIENTED_EDGE ( 'NONE', *, *, #7982, .F. ) ;
#8894 = CARTESIAN_POINT ( 'NONE',  ( 0.07214854559197284023, -0.5476281405333195407, 0.9202755905511811330 ) ) ;
#8895 = DIRECTION ( 'NONE',  ( 0.000000000000000000, 1.000000000000000000, 0.000000000000000000 ) ) ;
#8896 = EDGE_LOOP ( 'NONE', ( #15371, #7415, #19217, #22384 ) ) ;
#8897 = CARTESIAN_POINT ( 'NONE',  ( 0.4160174684701755665, 0.3320469875258716397, 0.1322810039474933141 ) ) ;
#8898 = DIRECTION ( 'NONE',  ( -1.000000000000000000, 0.000000000000000000, 0.000000000000000000 ) ) ;
#8899 = CARTESIAN_POINT ( 'NONE',  ( 0.3183792087432348872, -0.6629319518599616767, 0.2763636194390191592 ) ) ;
#8900 = EDGE_CURVE ( 'NONE', #24768, #5827, #12722, .T. ) ;
#8901 = EDGE_CURVE ( 'NONE', #6630, #17458, #20378, .T. ) ;
#8902 = FACE_BOUND ( 'NONE', #26860, .T. ) ;
#8903 = CARTESIAN_POINT ( 'NONE',  ( -0.1968503937007874127, 1.355271913027328057E-17, 0.1476377952755905387 ) ) ;
#8904 = CARTESIAN_POINT ( 'NONE',  ( -0.5905511811023621549, -0.4724409448818898127, 0.8182917201112815953 ) ) ;
#8905 = ORIENTED_EDGE ( 'NONE', *, *, #23315, .T. ) ;
#8906 = LINE ( 'NONE', #19923, #10954 ) ;
#8907 = CARTESIAN_POINT ( 'NONE',  ( 0.8558003517949211991, 0.6468501409757874132, 2.145669291338582862 ) ) ;
#8908 = AXIS2_PLACEMENT_3D ( 'NONE', #7959, #3853, #16560 ) ;
#8909 = AXIS2_PLACEMENT_3D ( 'NONE', #4860, #9661, #638 ) ;
#8910 = CARTESIAN_POINT ( 'NONE',  ( -0.09842519685039370636, 0.07874015748031495954, 0.04546065111729331171 ) ) ;
#8911 = PRODUCT_DEFINITION_SHAPE ( 'NONE', 'NONE',  #27895 ) ;
#8912 = DIRECTION ( 'NONE',  ( 1.000000000000000000, 0.000000000000000000, 0.000000000000000000 ) ) ;
#8913 = VERTEX_POINT ( 'NONE', #19651 ) ;
#8914 = CARTESIAN_POINT ( 'NONE',  ( 0.5118124425185632820, 0.03359157810808711259, -1.550196850393701142 ) ) ;
#8915 = ORIENTED_EDGE ( 'NONE', *, *, #15075, .T. ) ;
#8916 = EDGE_LOOP ( 'NONE', ( #26631, #368, #6675, #10235 ) ) ;
#8917 = EDGE_CURVE ( 'NONE', #13542, #25295, #14073, .T. ) ;
#8918 = CARTESIAN_POINT ( 'NONE',  ( -0.09139240964747707974, -0.07874015748031502893, 0.02109836160874977232 ) ) ;
#8919 = DIRECTION ( 'NONE',  ( 1.000000000000000000, 0.000000000000000000, 0.000000000000000000 ) ) ;
#8920 = LINE ( 'NONE', #10911, #3799 ) ;
#8921 = CARTESIAN_POINT ( 'NONE',  ( 0.3430989538749588119, 0.06100393589356664648, 0.1166443193823661489 ) ) ;
#8922 = VERTEX_POINT ( 'NONE', #6661 ) ;
#8923 = DIRECTION ( 'NONE',  ( 1.000000000000000000, 5.737213000000000442E-16, 0.000000000000000000 ) ) ;
#8924 = VERTEX_POINT ( 'NONE', #1988 ) ;
#8925 = CIRCLE ( 'NONE', #10275, 0.2256712916308122319 ) ;
#8926 = CARTESIAN_POINT ( 'NONE',  ( -0.1981752911889803348, -0.08335338672471442889, -0.2362204724409444623 ) ) ;
#8927 = AXIS2_PLACEMENT_3D ( 'NONE', #25679, #8981, #12948 ) ;
#8928 = PRESENTATION_LAYER_ASSIGNMENT (  '', '', ( #9349 ) ) ;
#8929 = CARTESIAN_POINT ( 'NONE',  ( 0.6867658503605201803, -0.1559616964378681969, 0.3281099440185237248 ) ) ;
#8930 = CARTESIAN_POINT ( 'NONE',  ( 0.3334645669291338987, -1.269546425348450747, -0.8304542831125020230 ) ) ;
#8931 = LENGTH_MEASURE_WITH_UNIT ( LENGTH_MEASURE( 0.02539999999999999897 ), #6965 ) ;
#8932 = CARTESIAN_POINT ( 'NONE',  ( -0.6299212598425196763, 0.5659448818897637734, 0.000000000000000000 ) ) ;
#8933 = CARTESIAN_POINT ( 'NONE',  ( -0.3937007873768824662, 4.821444090828918336E-17, -0.1377952755696461029 ) ) ;
#8934 = VERTEX_POINT ( 'NONE', #10748 ) ;
#8935 = AXIS2_PLACEMENT_3D ( 'NONE', #3102, #11316, #20357 ) ;
#8936 = DIRECTION ( 'NONE',  ( 1.000000000000000000, 0.000000000000000000, 0.000000000000000000 ) ) ;
#8937 = LINE ( 'NONE', #13584, #17969 ) ;
#8938 = CARTESIAN_POINT ( 'NONE',  ( 0.3979194638820595098, 0.2297883689023132170, -1.928289503579157183 ) ) ;
#8939 = TOROIDAL_SURFACE ( 'NONE', #13021, 0.6751968503937006982, 0.01377952755905511792 ) ;
#8940 = VECTOR ( 'NONE', #18515, 39.37007874015748143 ) ;
#8941 = CIRCLE ( 'NONE', #26515, 0.5322834645669292097 ) ;
#8942 = CARTESIAN_POINT ( 'NONE',  ( -0.6112138326843681302, -0.1413929495357376109, 0.06990500580186909119 ) ) ;
#8943 = DIRECTION ( 'NONE',  ( -0.9790454724845839563, 0.1018208755700888840, 0.1763589297585419768 ) ) ;
#8944 = EDGE_CURVE ( 'NONE', #25079, #2223, #545, .T. ) ;
#8945 = CARTESIAN_POINT ( 'NONE',  ( -0.4922996667774039437, 0.08741303158498453518, 0.1259302777225530801 ) ) ;
#8946 = EDGE_CURVE ( 'NONE', #6378, #8220, #16334, .T. ) ;
#8947 = CARTESIAN_POINT ( 'NONE',  ( -0.07874015748031495954, 0.01169115616675828022, -0.4660234066338417858 ) ) ;
#8948 = CARTESIAN_POINT ( 'NONE',  ( -0.4986013261500205074, 0.000000000000000000, -0.1033464566929133965 ) ) ;
#8949 = CARTESIAN_POINT ( 'NONE',  ( 0.4158785340170984557, 0.3322209827720822850, 0.3401591244667909186 ) ) ;
#8950 = ADVANCED_FACE ( 'NONE', ( #6795, #10887 ), #21351, .T. ) ;
#8951 = ORIENTED_EDGE ( 'NONE', *, *, #19728, .F. ) ;
#8952 = CARTESIAN_POINT ( 'NONE',  ( 0.3543307086614173596, 0.000000000000000000, 1.953740157480315043 ) ) ;
#8953 = ORIENTED_EDGE ( 'NONE', *, *, #22840, .F. ) ;
#8954 = CARTESIAN_POINT ( 'NONE',  ( -0.1968503937007874127, 0.07874015748031495954, -0.04546065111729338803 ) ) ;
#8955 = SPHERICAL_SURFACE ( 'NONE', #21055, 0.1003956692913385851 ) ;
#8956 = CARTESIAN_POINT ( 'NONE',  ( 0.000000000000000000, 0.5007874015748031704, 0.3059055118110236560 ) ) ;
#8957 = EDGE_CURVE ( 'NONE', #1755, #9314, #8361, .T. ) ;
#8958 = ADVANCED_FACE ( 'NONE', ( #8627 ), #8233, .F. ) ;
#8959 = DIRECTION ( 'NONE',  ( 0.000000000000000000, 0.000000000000000000, -1.000000000000000000 ) ) ;
#8960 = CARTESIAN_POINT ( 'NONE',  ( 1.197070535079588716, 0.07874015748031495954, 1.197070535079588716 ) ) ;
#8961 = VECTOR ( 'NONE', #8562, 39.37007874015748854 ) ;
#8962 = AXIS2_PLACEMENT_3D ( 'NONE', #18340, #23034, #14135 ) ;
#8963 = CARTESIAN_POINT ( 'NONE',  ( -0.2303471512294322787, -0.4798602677570401598, 0.3401574803149606252 ) ) ;
#8964 = CARTESIAN_POINT ( 'NONE',  ( -0.1200583359873055728, 0.3535721684717720859, -3.115157480314960647 ) ) ;
#8965 = AXIS2_PLACEMENT_3D ( 'NONE', #10400, #14533, #19018 ) ;
#8966 = CARTESIAN_POINT ( 'NONE',  ( -0.2428345617565149384, 0.2885915454824177218, 0.07637795275590551769 ) ) ;
#8967 = CARTESIAN_POINT ( 'NONE',  ( -7.608238775805210269E-17, -0.6212598425196850238, -3.278217716535432842E-17 ) ) ;
#8968 = ORIENTED_EDGE ( 'NONE', *, *, #10873, .F. ) ;
#8969 = FACE_OUTER_BOUND ( 'NONE', #16226, .T. ) ;
#8970 = ORIENTED_EDGE ( 'NONE', *, *, #1526, .F. ) ;
#8971 = CARTESIAN_POINT ( 'NONE',  ( -0.06200787401574805319, 7.593774443531818500E-18, -4.015748031496062964 ) ) ;
#8972 = CARTESIAN_POINT ( 'NONE',  ( 0.1339654526248285071, 0.4984899526255159308, 1.766732283464566899 ) ) ;
#8973 = APPLICATION_PROTOCOL_DEFINITION ( 'draft international standard', 'automotive_design', 1998, #20452 ) ;
#8974 = CARTESIAN_POINT ( 'NONE',  ( -0.3121994997598287469, 0.4069448477556107946, 1.766732283464566899 ) ) ;
#8975 = CARTESIAN_POINT ( 'NONE',  ( -0.2268096725222598919, -0.4600326175560532915, 1.747047244094488194 ) ) ;
#8976 = DIRECTION ( 'NONE',  ( 0.000000000000000000, 1.000000000000000000, 0.000000000000000000 ) ) ;
#8977 = ORIENTED_EDGE ( 'NONE', *, *, #10512, .T. ) ;
#8978 = EDGE_CURVE ( 'NONE', #14228, #4851, #27635, .T. ) ;
#8979 = ORIENTED_EDGE ( 'NONE', *, *, #20893, .T. ) ;
#8980 = AXIS2_PLACEMENT_3D ( 'NONE', #1239, #25235, #11676 ) ;
#8982 = CARTESIAN_POINT ( 'NONE',  ( 0.2272836761397900307, -0.2962590301041579388, -3.115157480314960647 ) ) ;
#8981 = DIRECTION ( 'NONE',  ( 0.000000000000000000, 0.000000000000000000, 1.000000000000000000 ) ) ;
#8983 = AXIS2_PLACEMENT_3D ( 'NONE', #12532, #18739, #27094 ) ;
#8984 = ORIENTED_EDGE ( 'NONE', *, *, #17167, .F. ) ;
#8985 = DIRECTION ( 'NONE',  ( 0.000000000000000000, -1.000000000000000000, 0.000000000000000000 ) ) ;
#8986 = CARTESIAN_POINT ( 'NONE',  ( -0.3334645669291338987, 0.000000000000000000, -1.052618110236220428 ) ) ;
#8987 = ADVANCED_FACE ( 'NONE', ( #25729 ), #23597, .F. ) ;
#8988 = CARTESIAN_POINT ( 'NONE',  ( 0.02190250779246093876, -0.3346456692913385988, 1.953740157480315043 ) ) ;
#8989 = VERTEX_POINT ( 'NONE', #15006 ) ;
#8990 = EDGE_LOOP ( 'NONE', ( #9299, #26916, #9353, #15904, #4549 ) ) ;
#8991 = B_SPLINE_CURVE_WITH_KNOTS ( 'NONE', 2,
 ( #24380, #5026, #13644 ),
 .UNSPECIFIED., .F., .F.,
 ( 3, 3 ),
 ( 0.000000000000000000, 1.000000000000000000 ),
 .UNSPECIFIED. ) ;
#8992 = CARTESIAN_POINT ( 'NONE',  ( 0.1522836969735572310, -0.4941010236220472751, 6.050992370341708321E-17 ) ) ;
#8993 = CARTESIAN_POINT ( 'NONE',  ( -0.1181102362204724532, 0.000000000000000000, 0.6299212598425196763 ) ) ;
#8994 = ADVANCED_FACE ( 'NONE', ( #25866 ), #22451, .T. ) ;
#8995 = ORIENTED_EDGE ( 'NONE', *, *, #26584, .F. ) ;
#8996 = EDGE_LOOP ( 'NONE', ( #15266, #11286 ) ) ;
#8997 = EDGE_LOOP ( 'NONE', ( #10401, #23349, #11388, #20610, #26136 ) ) ;
#8998 = FACE_OUTER_BOUND ( 'NONE', #13161, .T. ) ;
#8999 = DIRECTION ( 'NONE',  ( -1.000000000000000000, 0.000000000000000000, 0.000000000000000000 ) ) ;
#9000 = DIRECTION ( 'NONE',  ( -0.000000000000000000, 1.000000000000000000, 0.000000000000000000 ) ) ;
#9001 = EDGE_LOOP ( 'NONE', ( #23203, #5858, #9564, #12891, #560, #27568 ) ) ;
#9002 = AXIS2_PLACEMENT_3D ( 'NONE', #22796, #14331, #7691 ) ;
#9003 = EDGE_CURVE ( 'NONE', #23265, #21357, #14570, .T. ) ;
#9004 = AXIS2_PLACEMENT_3D ( 'NONE', #2330, #17589, #6863 ) ;
#9005 = FACE_OUTER_BOUND ( 'NONE', #6886, .T. ) ;
#9006 = CARTESIAN_POINT ( 'NONE',  ( -0.3149606299212598381, 3.857155272905049219E-17, -3.666338582670846780 ) ) ;
#9007 = ( NAMED_UNIT ( * ) PLANE_ANGLE_UNIT ( ) SI_UNIT ( $, .RADIAN. ) ) ;
#9008 = FACE_BOUND ( 'NONE', #9791, .T. ) ;
#9009 = CARTESIAN_POINT ( 'NONE',  ( 0.07874015748031495954, 0.02870816175736372669, -0.4702756685301184292 ) ) ;
#9010 = CARTESIAN_POINT ( 'NONE',  ( -4.821283464566928349E-18, 0.000000000000000000, -0.3779527559055118058 ) ) ;
#9011 = B_SPLINE_CURVE_WITH_KNOTS ( 'NONE', 3,
 ( #3282, #16303, #7253, #24905, #14192, #13751, #2858, #22794, #11496, #3418 ),
 .UNSPECIFIED., .F., .F.,
 ( 4, 2, 2, 2, 4 ),
 ( 0.000000000000000000, 0.2500000000000000000, 0.5000000000000000000, 0.7500000000000000000, 1.000000000000000000 ),
 .UNSPECIFIED. ) ;
#9012 = ADVANCED_FACE ( 'NONE', ( #7197 ), #18185, .F. ) ;
#9013 = VERTEX_POINT ( 'NONE', #18037 ) ;
#9014 = CARTESIAN_POINT ( 'NONE',  ( 0.4143458349581316535, -0.2398979215371937757, 0.08349695147638480641 ) ) ;
#9015 = VERTEX_POINT ( 'NONE', #26825 ) ;
#9016 = PLANE ( 'NONE',  #19562 ) ;
#9017 = ADVANCED_FACE ( 'NONE', ( #2537 ), #11381, .F. ) ;
#9018 = VECTOR ( 'NONE', #26167, 39.37007874015748854 ) ;
#9019 = ORIENTED_EDGE ( 'NONE', *, *, #26613, .T. ) ;
#9020 = CARTESIAN_POINT ( 'NONE',  ( -0.009795313329799356164, 0.08526597544922019656, -0.4724409448841456749 ) ) ;
#9021 = VECTOR ( 'NONE', #22881, 39.37007874015748854 ) ;
#9022 = CARTESIAN_POINT ( 'NONE',  ( -1.692913385826771533, 0.07874015748031491790, -1.036610629921259805E-16 ) ) ;
#9023 = CARTESIAN_POINT ( 'NONE',  ( -0.3606049308155347410, 0.06410376196632514012, 0.08455817587594735563 ) ) ;
#9024 = DIRECTION ( 'NONE',  ( 0.000000000000000000, 0.000000000000000000, 1.000000000000000000 ) ) ;
#9025 = VERTEX_POINT ( 'NONE', #26403 ) ;
#9026 = CARTESIAN_POINT ( 'NONE',  ( -0.1429116519061139623, 0.5335524835332415838, 0.9399606299212598381 ) ) ;
#9027 = EDGE_LOOP ( 'NONE', ( #2348, #1849, #26966, #5414 ) ) ;
#9028 = DIRECTION ( 'NONE',  ( 1.000000000000000000, 0.000000000000000000, 0.000000000000000000 ) ) ;
#9029 = ORIENTED_EDGE ( 'NONE', *, *, #24577, .F. ) ;
#9030 = FILL_AREA_STYLE_COLOUR ( '', #4143 ) ;
#9031 = CARTESIAN_POINT ( 'NONE',  ( 0.0004447986960614961401, 0.5322833254990984031, 0.3401591244667909186 ) ) ;
#9032 = DIRECTION ( 'NONE',  ( 0.5000000010362839475, -0.8660254031861397417, 1.060575237992202059E-16 ) ) ;
#9033 = CARTESIAN_POINT ( 'NONE',  ( -0.6299212598425196763, 0.9448818897637796255, -0.1771653543307086520 ) ) ;
#9034 = LINE ( 'NONE', #11710, #25362 ) ;
#9035 = CARTESIAN_POINT ( 'NONE',  ( 0.000000000000000000, 0.000000000000000000, 0.09685039370078740717 ) ) ;
#9036 = EDGE_CURVE ( 'NONE', #21231, #1085, #5978, .T. ) ;
#9037 = CARTESIAN_POINT ( 'NONE',  ( -0.0004974201395674843510, 0.3464563358313494934, 0.1478915661211720467 ) ) ;
#9038 = CARTESIAN_POINT ( 'NONE',  ( 0.4620608682196457040, 0.08206165078054626638, 0.07637795275590551769 ) ) ;
#9039 = CARTESIAN_POINT ( 'NONE',  ( -0.3661417322834645272, -0.4724409448818898127, 0.6411263657805729155 ) ) ;
#9040 = CARTESIAN_POINT ( 'NONE',  ( -0.2425693455392318731, 0.2888145544500153594, 0.07637549214372854611 ) ) ;
#9041 = ORIENTED_EDGE ( 'NONE', *, *, #6155, .T. ) ;
#9042 = CYLINDRICAL_SURFACE ( 'NONE', #6908, 0.4010740433761567081 ) ;
#9043 = CARTESIAN_POINT ( 'NONE',  ( -0.3218517393633636980, 0.3826375019116435294, 0.1259302777250448369 ) ) ;
#9044 = CARTESIAN_POINT ( 'NONE',  ( -0.4954156765914849991, -0.2860899518037616773, 0.9399606299212598381 ) ) ;
#9045 = CARTESIAN_POINT ( 'NONE',  ( -0.4472135058506043759, -0.2577577458591217008, 1.766732283464566677 ) ) ;
#9046 = CARTESIAN_POINT ( 'NONE',  ( -0.09842519685039366473, 0.1968503937007873850, -3.548228346456693050 ) ) ;
#9047 = CARTESIAN_POINT ( 'NONE',  ( -0.5118110236220472231, 0.000000000000000000, -0.1377952755905511861 ) ) ;
#9048 = EDGE_CURVE ( 'NONE', #19937, #24839, #3722, .T. ) ;
#9049 = AXIS2_PLACEMENT_3D ( 'NONE', #10830, #7010, #19445 ) ;
#9050 = ORIENTED_EDGE ( 'NONE', *, *, #5186, .F. ) ;
#9051 = EDGE_CURVE ( 'NONE', #25393, #11604, #15026, .T. ) ;
#9052 = ORIENTED_EDGE ( 'NONE', *, *, #11372, .T. ) ;
#9053 = CARTESIAN_POINT ( 'NONE',  ( -0.4055118110236220486, -0.4724409448818898127, 0.6874452634183660926 ) ) ;
#9054 = DIRECTION ( 'NONE',  ( 0.000000000000000000, 0.000000000000000000, -1.000000000000000000 ) ) ;
#9055 = DIRECTION ( 'NONE',  ( -1.000000000000000000, 0.000000000000000000, 0.000000000000000000 ) ) ;
#9056 = APPLICATION_CONTEXT ( 'automotive_design' ) ;
#9057 = EDGE_LOOP ( 'NONE', ( #9907, #2276, #10800, #14077 ) ) ;
#9058 = CARTESIAN_POINT ( 'NONE',  ( -0.6614173228346456046, 0.000000000000000000, -0.1309055118110236116 ) ) ;
#9059 = ORIENTED_EDGE ( 'NONE', *, *, #26368, .T. ) ;
#9060 = CARTESIAN_POINT ( 'NONE',  ( -0.2165354330708661457, 0.000000000000000000, 0.000000000000000000 ) ) ;
#9061 = CIRCLE ( 'NONE', #5004, 0.7500000000000001110 ) ;
#9062 = CARTESIAN_POINT ( 'NONE',  ( -0.5383572925356228112, -0.3100567972183445042, 0.2574803149606298969 ) ) ;
#9063 = CARTESIAN_POINT ( 'NONE',  ( 0.4895462770358314786, 0.9151958316345965017, -0.3874954751611386361 ) ) ;
#9064 = DIRECTION ( 'NONE',  ( -0.000000000000000000, 1.000000000000000000, -0.000000000000000000 ) ) ;
#9065 = AXIS2_PLACEMENT_3D ( 'NONE', #17901, #843, #24554 ) ;
#9066 = VECTOR ( 'NONE', #24497, 39.37007874015748143 ) ;
#9067 = DIRECTION ( 'NONE',  ( 0.000000000000000000, 0.000000000000000000, 1.000000000000000000 ) ) ;
#9068 = EDGE_LOOP ( 'NONE', ( #15802, #5351 ) ) ;
#9069 = DIRECTION ( 'NONE',  ( 0.000000000000000000, 0.000000000000000000, 1.000000000000000000 ) ) ;
#9070 = CARTESIAN_POINT ( 'NONE',  ( 0.3707612262533033776, -0.3252100150720387273, -1.550196850393700920 ) ) ;
#9071 = CARTESIAN_POINT ( 'NONE',  ( -0.1188866373884876204, 0.4438564651657459503, -1.928289503579154740 ) ) ;
#9072 = ORIENTED_EDGE ( 'NONE', *, *, #11218, .T. ) ;
#9073 = CARTESIAN_POINT ( 'NONE',  ( 0.000000000000000000, 0.000000000000000000, 0.1377952755905511861 ) ) ;
#9074 = CARTESIAN_POINT ( 'NONE',  ( 0.3200513472073915344, 0.3804946224884545591, 0.1615162260904031422 ) ) ;
#9075 = CARTESIAN_POINT ( 'NONE',  ( -0.0006345105826669221114, 0.4803145415259080231, 0.2194422276343239164 ) ) ;
#9076 = CIRCLE ( 'NONE', #19010, 0.4692913385826771866 ) ;
#9077 = DIRECTION ( 'NONE',  ( 0.4338837391175581204, 0.9009688679024192570, -0.000000000000000000 ) ) ;
#9078 = FACE_OUTER_BOUND ( 'NONE', #21718, .T. ) ;
#9079 = EDGE_CURVE ( 'NONE', #7941, #17590, #25838, .T. ) ;
#9080 = CIRCLE ( 'NONE', #2764, 0.3872945158171015589 ) ;
#9081 = AXIS2_PLACEMENT_3D ( 'NONE', #24752, #16007, #24461 ) ;
#9082 = CARTESIAN_POINT ( 'NONE',  ( 0.000000000000000000, -1.446320346059429855E-17, 0.1181010187644645215 ) ) ;
#9083 = CARTESIAN_POINT ( 'NONE',  ( 0.09590060490395689585, 0.1136516277932340530, -0.1968503937007874127 ) ) ;
#9084 = ORIENTED_EDGE ( 'NONE', *, *, #22356, .F. ) ;
#9085 = LINE ( 'NONE', #761, #4626 ) ;
#9086 = LINE ( 'NONE', #17702, #27247 ) ;
#9087 = CARTESIAN_POINT ( 'NONE',  ( -0.6562077975700097987, -9.864972440944882481E-14, 0.2362204724409449064 ) ) ;
#9088 = ORIENTED_EDGE ( 'NONE', *, *, #25383, .T. ) ;
#9089 = CARTESIAN_POINT ( 'NONE',  ( -0.4382752542996525835, 0.1173917140416343985, -1.934055118110236338 ) ) ;
#9090 = DIRECTION ( 'NONE',  ( -1.000000000000000000, 0.000000000000000000, -0.000000000000000000 ) ) ;
#9091 = DIRECTION ( 'NONE',  ( 0.000000000000000000, 0.000000000000000000, 1.000000000000000000 ) ) ;
#9092 = CARTESIAN_POINT ( 'NONE',  ( -0.2602238532265429005, 0.000000000000000000, 0.2362204724409449064 ) ) ;
#9093 = VECTOR ( 'NONE', #15177, 39.37007874015748143 ) ;
#9094 = DIRECTION ( 'NONE',  ( 0.000000000000000000, 1.000000000000000000, 0.000000000000000000 ) ) ;
#9095 = CARTESIAN_POINT ( 'NONE',  ( 0.3384212623783103835, 0.1668516812751408562, -3.100567304031765392 ) ) ;
#9096 = DIRECTION ( 'NONE',  ( -0.5000000000000009992, 6.123233995736778362E-17, 0.8660254037844380415 ) ) ;
#9097 = CARTESIAN_POINT ( 'NONE',  ( -2.073220866141732523E-16, 0.07874015748031491790, 1.574803149606299524 ) ) ;
#9098 = CARTESIAN_POINT ( 'NONE',  ( 0.1512365935307563025, 0.2842733266362078570, 0.3980489158656032589 ) ) ;
#9099 = EDGE_CURVE ( 'NONE', #25691, #18857, #13634, .T. ) ;
#9100 = EDGE_LOOP ( 'NONE', ( #16327, #10744, #13790, #23170 ) ) ;
#9101 = EDGE_CURVE ( 'NONE', #7057, #1086, #9034, .T. ) ;
#9102 = SPHERICAL_SURFACE ( 'NONE', #16835, 0.07677362204724409722 ) ;
#9103 = AXIS2_PLACEMENT_3D ( 'NONE', #27366, #7201, #10119 ) ;
#9104 = ORIENTED_EDGE ( 'NONE', *, *, #24328, .F. ) ;
#9105 = EDGE_CURVE ( 'NONE', #13078, #16461, #7337, .T. ) ;
#9106 = DIRECTION ( 'NONE',  ( 0.000000000000000000, 0.000000000000000000, 1.000000000000000000 ) ) ;
#9107 = CARTESIAN_POINT ( 'NONE',  ( -0.3346456692913385988, 0.000000000000000000, 2.504921259842519898 ) ) ;
#9108 = PRODUCT_CONTEXT ( 'NONE', #22809, 'mechanical' ) ;
#9109 = CARTESIAN_POINT ( 'NONE',  ( 0.5085118447801426633, -0.06699507805369582514, 1.766732283464566899 ) ) ;
#9110 = B_SPLINE_CURVE_WITH_KNOTS ( 'NONE', 3,
 ( #25935, #385, #2601, #4326, #6728, #8966 ),
 .UNSPECIFIED., .F., .F.,
 ( 4, 2, 4 ),
 ( 0.5000000000000000000, 0.7500000000000000000, 1.000000000000000000 ),
 .UNSPECIFIED. ) ;
#9111 = SURFACE_SIDE_STYLE ('',( #17334 ) ) ;
#9112 = VECTOR ( 'NONE', #6719, 39.37007874015748143 ) ;
#9113 = CARTESIAN_POINT ( 'NONE',  ( -0.02438677169350799909, 0.3726024258163779246, -3.115157480314960647 ) ) ;
#9114 = ORIENTED_EDGE ( 'NONE', *, *, #2966, .F. ) ;
#9115 = CARTESIAN_POINT ( 'NONE',  ( -0.5377323685532543474, 0.4294741335735771659, 0.3401591245381555551 ) ) ;
#9116 = DIRECTION ( 'NONE',  ( 1.000000000000000000, 0.000000000000000000, 0.000000000000000000 ) ) ;
#9117 = CARTESIAN_POINT ( 'NONE',  ( 0.1677079028045370679, 0.2904160862623488826, 1.953740157480315043 ) ) ;
#9118 = ORIENTED_EDGE ( 'NONE', *, *, #27438, .F. ) ;
#9119 = VERTEX_POINT ( 'NONE', #24158 ) ;
#9120 = ORIENTED_EDGE ( 'NONE', *, *, #21396, .T. ) ;
#9121 = AXIS2_PLACEMENT_3D ( 'NONE', #12706, #27560, #6093 ) ;
#9122 = CYLINDRICAL_SURFACE ( 'NONE', #1048, 0.1308464566929133932 ) ;
#9123 = ORIENTED_EDGE ( 'NONE', *, *, #22606, .F. ) ;
#9124 = EDGE_LOOP ( 'NONE', ( #23149, #2087, #10454, #5204, #27581, #11490, #20748, #695 ) ) ;
#9125 = ORIENTED_EDGE ( 'NONE', *, *, #4983, .T. ) ;
#9126 = CARTESIAN_POINT ( 'NONE',  ( -0.06294778803469826267, 0.1968503937007874127, -3.596639928719705281 ) ) ;
#9127 = ADVANCED_FACE ( 'NONE', ( #13689 ), #16355, .T. ) ;
#9128 = CARTESIAN_POINT ( 'NONE',  ( 0.4898768902087983768, -3.758337795275590876E-16, 0.07874015748031495954 ) ) ;
#9129 = CARTESIAN_POINT ( 'NONE',  ( -0.3048711895205613587, -0.6348424542980738439, 0.3281099440176195592 ) ) ;
#9130 = CARTESIAN_POINT ( 'NONE',  ( 0.7611552401864779549, 0.5997378224220212273, 0.08818015398314092701 ) ) ;
#9131 = ORIENTED_EDGE ( 'NONE', *, *, #25291, .F. ) ;
#9132 = AXIS2_PLACEMENT_3D ( 'NONE', #11912, #18387, #22509 ) ;
#9133 = ADVANCED_FACE ( 'NONE', ( #13282 ), #4179, .T. ) ;
#9134 = AXIS2_PLACEMENT_3D ( 'NONE', #23819, #8695, #19848 ) ;
#9135 = FACE_OUTER_BOUND ( 'NONE', #8112, .T. ) ;
#9136 = ADVANCED_FACE ( 'NONE', ( #447 ), #20865, .F. ) ;
#9137 = CARTESIAN_POINT ( 'NONE',  ( -0.2669480828848088128, -0.2341512108694275007, 1.953740157480315043 ) ) ;
#9138 = EDGE_CURVE ( 'NONE', #26345, #4501, #17651, .T. ) ;
#9139 = CARTESIAN_POINT ( 'NONE',  ( -0.0006568023596623034704, 0.5148705051068777072, 0.3251195115599746499 ) ) ;
#9140 = AXIS2_PLACEMENT_3D ( 'NONE', #27584, #1998, #18949 ) ;
#9141 = DIRECTION ( 'NONE',  ( 0.000000000000000000, 1.000000000000000000, 0.000000000000000000 ) ) ;
#9142 = ADVANCED_FACE ( 'NONE', ( #2940 ), #10928, .T. ) ;
#9143 = CARTESIAN_POINT ( 'NONE',  ( -0.4009292313423786780, -0.2321359940675791766, 0.2048502514806590791 ) ) ;
#9144 = CARTESIAN_POINT ( 'NONE',  ( -0.5949363243629232079, -0.1357903337134990229, 0.2362204724409449064 ) ) ;
#9145 = LINE ( 'NONE', #15666, #295 ) ;
#9146 = ORIENTED_EDGE ( 'NONE', *, *, #13195, .T. ) ;
#9147 = CARTESIAN_POINT ( 'NONE',  ( 0.6055690743987126590, 0.2581485381169802973, 0.4471263839182408883 ) ) ;
#9148 = AXIS2_PLACEMENT_3D ( 'NONE', #12266, #8450, #5926 ) ;
#9149 = EDGE_LOOP ( 'NONE', ( #26444, #21592, #9088, #24473 ) ) ;
#9150 = LINE ( 'NONE', #17770, #7170 ) ;
#9151 = EDGE_LOOP ( 'NONE', ( #9394, #21259, #4346, #2928 ) ) ;
#9152 = ORIENTED_EDGE ( 'NONE', *, *, #26098, .T. ) ;
#9153 = ORIENTED_EDGE ( 'NONE', *, *, #355, .T. ) ;
#9154 = CIRCLE ( 'NONE', #24494, 0.1181102362204720091 ) ;
#9155 = DIRECTION ( 'NONE',  ( 0.000000000000000000, 1.000000000000000000, 0.000000000000000000 ) ) ;
#9156 = CARTESIAN_POINT ( 'NONE',  ( 0.3149606299212598381, 3.857155272905049219E-17, -0.03543307086614173179 ) ) ;
#9157 = EDGE_LOOP ( 'NONE', ( #18455, #8245 ) ) ;
#9158 = CARTESIAN_POINT ( 'NONE',  ( 0.4382482975805209735, 0.3362148458989007715, 0.9399606299212598381 ) ) ;
#9159 = TOROIDAL_SURFACE ( 'NONE', #15501, 0.5915354330708662012, 0.05216535433070866590 ) ;
#9160 = CARTESIAN_POINT ( 'NONE',  ( 0.000000000000000000, 0.000000000000000000, 0.1992125984251968684 ) ) ;
#9161 = CARTESIAN_POINT ( 'NONE',  ( 0.1257482708759803669, -0.3439950301957984680, 0.08455817587492829579 ) ) ;
#9162 = DIRECTION ( 'NONE',  ( 0.000000000000000000, -1.000000000000000000, 0.000000000000000000 ) ) ;
#9163 = AXIS2_PLACEMENT_3D ( 'NONE', #3188, #18008, #9699 ) ;
#9164 = CARTESIAN_POINT ( 'NONE',  ( -0.1968503937007874127, 0.07874015748031495954, -0.04546065111729338803 ) ) ;
#9165 = CARTESIAN_POINT ( 'NONE',  ( 0.000000000000000000, 0.000000000000000000, 0.4488188976377953110 ) ) ;
#9166 = CARTESIAN_POINT ( 'NONE',  ( 0.3346456692913385988, 0.000000000000000000, 1.953740157480315043 ) ) ;
#9167 = ADVANCED_FACE ( 'NONE', ( #11299 ), #15898, .F. ) ;
#9168 = CARTESIAN_POINT ( 'NONE',  ( 0.1490609433615242285, 0.000000000000000000, 0.000000000000000000 ) ) ;
#9169 = CARTESIAN_POINT ( 'NONE',  ( 0.4834654033848707622, -0.1110087727129997481, 0.2989974301291331016 ) ) ;
#9170 = CARTESIAN_POINT ( 'NONE',  ( -0.3175540113612215221, -0.1078280746903921422, 1.953740157480315043 ) ) ;
#9171 = EDGE_CURVE ( 'NONE', #25145, #6614, #164, .T. ) ;
#9172 = DIRECTION ( 'NONE',  ( 0.000000000000000000, 0.000000000000000000, 1.000000000000000000 ) ) ;
#9173 = CARTESIAN_POINT ( 'NONE',  ( 0.000000000000000000, 0.8661417322803149910, 0.000000000000000000 ) ) ;
#9174 = DIRECTION ( 'NONE',  ( 0.000000000000000000, 1.000000000000000000, 0.000000000000000000 ) ) ;
#9175 = CARTESIAN_POINT ( 'NONE',  ( -0.4890020181336406924, -0.1109469068267769365, 0.3080453759532011393 ) ) ;
#9176 = CARTESIAN_POINT ( 'NONE',  ( 0.5118110236220473341, 6.402768735150616610E-17, -1.550196850393700920 ) ) ;
#9177 = AXIS2_PLACEMENT_3D ( 'NONE', #13385, #4508, #13115 ) ;
#9178 = ORIENTED_EDGE ( 'NONE', *, *, #2293, .F. ) ;
#9179 = AXIS2_PLACEMENT_3D ( 'NONE', #15657, #5040, #4903 ) ;
#9180 = ADVANCED_FACE ( 'NONE', ( #16661 ), #16805, .F. ) ;
#9181 = ORIENTED_EDGE ( 'NONE', *, *, #23103, .F. ) ;
#9182 = FACE_OUTER_BOUND ( 'NONE', #21750, .T. ) ;
#9183 = CARTESIAN_POINT ( 'NONE',  ( 0.3334645669291338987, -1.269546425348450747, -0.8304542831125020230 ) ) ;
#9184 = EDGE_LOOP ( 'NONE', ( #8786, #18721 ) ) ;
#9185 = VECTOR ( 'NONE', #23365, 39.37007874015748143 ) ;
#9186 = CARTESIAN_POINT ( 'NONE',  ( -0.1141732283464566844, 0.000000000000000000, 0.000000000000000000 ) ) ;
#9187 = ORIENTED_EDGE ( 'NONE', *, *, #615, .F. ) ;
#9188 = SHAPE_REPRESENTATION ( 'ISO 4762 M5x16 Socket Head Cap Screw', ( #11588, #27978, #27991, #28004 ), #3473 ) ;
#9189 = B_SPLINE_CURVE_WITH_KNOTS ( 'NONE', 3,
 ( #3259, #16002, #24889, #20519, #16147, #10053, #24745, #1176 ),
 .UNSPECIFIED., .F., .F.,
 ( 4, 2, 2, 4 ),
 ( 5.336250286684417789E-07, 0.0004434172983717937842, 0.0008863009717149190544, 0.001772068318401169270 ),
 .UNSPECIFIED. ) ;
#9190 = SURFACE_STYLE_FILL_AREA ( #5241 ) ;
#9191 = CARTESIAN_POINT ( 'NONE',  ( 0.6711032387266713251, -0.1523958994812761869, 0.3401574803149606252 ) ) ;
#9192 = CARTESIAN_POINT ( 'NONE',  ( 0.7871730179869745880, 0.2552990454435328793, -0.2788231443339960758 ) ) ;
#9193 = CARTESIAN_POINT ( 'NONE',  ( -0.4585215200179055817, 2.807634559150536355E-17, -1.928289503579156516 ) ) ;
#9194 = DIRECTION ( 'NONE',  ( 1.000000000000000000, 0.000000000000000000, 0.000000000000000000 ) ) ;
#9195 = ADVANCED_FACE ( 'NONE', ( #25127 ), #24847, .F. ) ;
#9196 = CIRCLE ( 'NONE', #4269, 0.2952755905511805778 ) ;
#9197 = ORIENTED_EDGE ( 'NONE', *, *, #16116, .F. ) ;
#9198 = CARTESIAN_POINT ( 'NONE',  ( -0.4211031283167419592, -0.2438048970097803081, 0.1827409795204104903 ) ) ;
#9199 = EDGE_CURVE ( 'NONE', #24937, #12967, #3019, .T. ) ;
#9200 = CARTESIAN_POINT ( 'NONE',  ( -0.2031943647053778002, -0.4121342552748231136, -1.928289503579173614 ) ) ;
#9201 = DIRECTION ( 'NONE',  ( 0.000000000000000000, 0.000000000000000000, 1.000000000000000000 ) ) ;
#9202 = CARTESIAN_POINT ( 'NONE',  ( 0.000000000000000000, 0.000000000000000000, 0.2637795275590551491 ) ) ;
#9203 = PLANE ( 'NONE',  #5125 ) ;
#9204 = CIRCLE ( 'NONE', #2890, 0.5007874015748031704 ) ;
#9205 = FACE_BOUND ( 'NONE', #20169, .T. ) ;
#9206 = CARTESIAN_POINT ( 'NONE',  ( -0.6434710025615986151, -0.04612040742723353542, 0.2355049364185476390 ) ) ;
#9207 = CARTESIAN_POINT ( 'NONE',  ( 0.2983664441502653641, -0.6201464311010354002, 0.3401599409343967761 ) ) ;
#9208 = ( LENGTH_UNIT ( ) NAMED_UNIT ( * ) SI_UNIT ( $, .METRE. ) ) ;
#9209 = DIRECTION ( 'NONE',  ( 0.000000000000000000, 0.000000000000000000, 1.000000000000000000 ) ) ;
#9210 = EDGE_CURVE ( 'NONE', #10703, #5544, #15462, .T. ) ;
#9211 = CIRCLE ( 'NONE', #3814, 0.3771653543307086909 ) ;
#9212 = DIRECTION ( 'NONE',  ( 0.000000000000000000, 0.000000000000000000, 1.000000000000000000 ) ) ;
#9213 = CONICAL_SURFACE ( 'NONE', #24123, 0.1074461786882927178, 1.047197550000000144 ) ;
#9214 = FACE_OUTER_BOUND ( 'NONE', #21386, .T. ) ;
#9215 = FACE_OUTER_BOUND ( 'NONE', #14839, .T. ) ;
#9216 = VERTEX_POINT ( 'NONE', #8052 ) ;
#9217 = DIRECTION ( 'NONE',  ( 0.000000000000000000, 0.000000000000000000, 1.000000000000000000 ) ) ;
#9218 = ORIENTED_EDGE ( 'NONE', *, *, #5424, .T. ) ;
#9219 = CARTESIAN_POINT ( 'NONE',  ( 0.3411003281197161341, 0.2991932138496539162, -1.934055118110236338 ) ) ;
#9220 = DIRECTION ( 'NONE',  ( 0.000000000000000000, 1.000000000000000000, 0.000000000000000000 ) ) ;
#9221 = CARTESIAN_POINT ( 'NONE',  ( 0.5188885761056504231, -0.1186607836835328750, 0.1322810039474935084 ) ) ;
#9222 = DIRECTION ( 'NONE',  ( 1.000000000000000000, 0.000000000000000000, 0.000000000000000000 ) ) ;
#9223 = AXIS2_PLACEMENT_3D ( 'NONE', #14251, #27097, #12249 ) ;
#9224 = CARTESIAN_POINT ( 'NONE',  ( -0.2228021814306022086, -0.4641672719493093457, 0.3251195115408473946 ) ) ;
#9225 = CARTESIAN_POINT ( 'NONE',  ( 0.2836590635674658412, -0.2488091035916875082, -3.100567304031767168 ) ) ;
#9226 = DIRECTION ( 'NONE',  ( 0.000000000000000000, 0.000000000000000000, 1.000000000000000000 ) ) ;
#9227 = FACE_OUTER_BOUND ( 'NONE', #8847, .T. ) ;
#9228 = ADVANCED_FACE ( 'NONE', ( #14417 ), #18473, .T. ) ;
#9229 = ORIENTED_EDGE ( 'NONE', *, *, #12850, .F. ) ;
#9230 = DIRECTION ( 'NONE',  ( 0.000000000000000000, 0.000000000000000000, -1.000000000000000000 ) ) ;
#9231 = EDGE_CURVE ( 'NONE', #1804, #8934, #11449, .T. ) ;
#9232 = AXIS2_PLACEMENT_3D ( 'NONE', #14485, #21352, #16444 ) ;
#9234 = CARTESIAN_POINT ( 'NONE',  ( -0.0002199787722624904878, 0.6212598425196850238, 0.2574827755769819038 ) ) ;
#9235 = ORIENTED_EDGE ( 'NONE', *, *, #18442, .F. ) ;
#9236 = CARTESIAN_POINT ( 'NONE',  ( -0.4164331889188472857, 0.3315254675241992577, 0.1322818204150988386 ) ) ;
#9237 = CARTESIAN_POINT ( 'NONE',  ( 0.000000000000000000, 0.000000000000000000, -4.330708661396418080 ) ) ;
#9238 = DIMENSIONAL_EXPONENTS ( 1.000000000000000000, 0.000000000000000000, 0.000000000000000000, 0.000000000000000000, 0.000000000000000000, 0.000000000000000000, 0.000000000000000000 ) ;
#9239 = CARTESIAN_POINT ( 'NONE',  ( -0.06699507805371239522, -0.5085118447801502128, 1.747047244094488194 ) ) ;
#9240 = DIRECTION ( 'NONE',  ( 0.000000000000000000, 0.000000000000000000, -1.000000000000000000 ) ) ;
#9241 = CARTESIAN_POINT ( 'NONE',  ( 0.1200583359873109851, -0.3535721684717733071, -3.115157480314960647 ) ) ;
#9242 = CARTESIAN_POINT ( 'NONE',  ( -1.928513779527558736E-17, 0.000000000000000000, -0.03543307086614173179 ) ) ;
#9243 = CARTESIAN_POINT ( 'NONE',  ( -4.821444091131312140E-17, -0.3937007874015748254, 0.4488188976377953110 ) ) ;
#9244 = CARTESIAN_POINT ( 'NONE',  ( -0.2660793235464293804, -0.2041304421298503202, 1.953740157480315043 ) ) ;
#9245 = ORIENTED_EDGE ( 'NONE', *, *, #4024, .F. ) ;
#9246 = ORIENTED_EDGE ( 'NONE', *, *, #14281, .T. ) ;
#9248 = ADVANCED_FACE ( 'NONE', ( #14122 ), #23161, .T. ) ;
#9247 = ORIENTED_EDGE ( 'NONE', *, *, #7229, .T. ) ;
#9249 = VERTEX_POINT ( 'NONE', #3217 ) ;
#9250 = CARTESIAN_POINT ( 'NONE',  ( 0.000000000000000000, 0.000000000000000000, 0.6299212598425196763 ) ) ;
#9251 = CIRCLE ( 'NONE', #24161, 0.8162224727389330026 ) ;
#9252 = ORIENTED_EDGE ( 'NONE', *, *, #25493, .F. ) ;
#9253 = ORIENTED_EDGE ( 'NONE', *, *, #27347, .T. ) ;
#9254 = VERTEX_POINT ( 'NONE', #20895 ) ;
#9255 = DIRECTION ( 'NONE',  ( 0.000000000000000000, 0.000000000000000000, 1.000000000000000000 ) ) ;
#9256 = AXIS2_PLACEMENT_3D ( 'NONE', #8948, #15473, #2585 ) ;
#9257 = EDGE_CURVE ( 'NONE', #27168, #14000, #27400, .T. ) ;
#9258 = ADVANCED_FACE ( 'NONE', ( #16380 ), #7625, .T. ) ;
#9259 = CARTESIAN_POINT ( 'NONE',  ( -0.3574975638436101444, 0.02339816079122976691, -3.115157480314960647 ) ) ;
#9260 = DIRECTION ( 'NONE',  ( 0.000000000000000000, -1.000000000000000000, 0.000000000000000000 ) ) ;
#9261 = CARTESIAN_POINT ( 'NONE',  ( -9.506830708661417994E-16, 0.000000000000000000, 0.000000000000000000 ) ) ;
#9262 = CARTESIAN_POINT ( 'NONE',  ( 0.6667153566691432776, 0.8231464062114414171, -0.06035729286437391955 ) ) ;
#9263 = AXIS2_PLACEMENT_3D ( 'NONE', #13459, #6985, #4842 ) ;
#9264 = CARTESIAN_POINT ( 'NONE',  ( -0.01288382813972197179, 0.2165354330708661734, -3.174212598425197207 ) ) ;
#9265 = CARTESIAN_POINT ( 'NONE',  ( -0.09187177619658884464, -0.3429980251342297226, 1.953740157480315043 ) ) ;
#9266 = DIRECTION ( 'NONE',  ( 0.000000000000000000, 1.000000000000000000, 0.000000000000000000 ) ) ;
#9267 = DIRECTION ( 'NONE',  ( 1.000000000000000000, 0.000000000000000000, 0.000000000000000000 ) ) ;
#9268 = CARTESIAN_POINT ( 'NONE',  ( -2.685748425196850164E-17, 0.000000000000000000, -1.934055118110236338 ) ) ;
#9269 = AXIS2_PLACEMENT_3D ( 'NONE', #7324, #694, #2527 ) ;
#9270 = B_SPLINE_CURVE_WITH_KNOTS ( 'NONE', 3,
 ( #25444, #8359, #10169, #20643, #3975, #25011 ),
 .UNSPECIFIED., .F., .F.,
 ( 4, 2, 4 ),
 ( 1.217380381967462011, 1.219305002860848086, 1.221229623754231941 ),
 .UNSPECIFIED. ) ;
#9271 = DIRECTION ( 'NONE',  ( 1.000000000000000000, 0.000000000000000000, 0.000000000000000000 ) ) ;
#9272 = CARTESIAN_POINT ( 'NONE',  ( -1.197070535079588716, 0.07874015748031491790, 1.078960298859116707 ) ) ;
#9273 = VECTOR ( 'NONE', #22934, 39.37007874015748143 ) ;
#9274 = DIRECTION ( 'NONE',  ( -0.4338837391175581204, 0.9009688679024192570, 0.000000000000000000 ) ) ;
#9275 = ORIENTED_EDGE ( 'NONE', *, *, #6471, .T. ) ;
#9276 = CARTESIAN_POINT ( 'NONE',  ( 0.4029514798603574532, 0.3205030004498418683, 0.1473214333212670424 ) ) ;
#9277 = CARTESIAN_POINT ( 'NONE',  ( -0.3214446924536846772, 0.3840069416942866742, 0.2574803149606298969 ) ) ;
#9278 = CARTESIAN_POINT ( 'NONE',  ( 0.1570773243920708662, -0.3184597017670454666, 1.953740157480315043 ) ) ;
#9279 = ORIENTED_EDGE ( 'NONE', *, *, #17358, .F. ) ;
#9280 = CARTESIAN_POINT ( 'NONE',  ( -0.4925073816770652591, 0.08623502184940523563, 0.1496602734601975015 ) ) ;
#9281 = EDGE_CURVE ( 'NONE', #25040, #20898, #182, .T. ) ;
#9282 = ORIENTED_EDGE ( 'NONE', *, *, #18108, .F. ) ;
#9283 = CARTESIAN_POINT ( 'NONE',  ( -0.2647715730835492609, -0.5498038367121063086, 0.2362204724409449064 ) ) ;
#9284 = CARTESIAN_POINT ( 'NONE',  ( 0.6707652279343347956, -0.1538768215240155779, 0.3401574803149606252 ) ) ;
#9285 = EDGE_LOOP ( 'NONE', ( #23979, #22439, #19635, #1175 ) ) ;
#9286 = CARTESIAN_POINT ( 'NONE',  ( 0.5417097841048850171, 0.1839420097223152528, 0.9399606299212598381 ) ) ;
#9287 = ORIENTED_EDGE ( 'NONE', *, *, #21474, .F. ) ;
#9288 = EDGE_CURVE ( 'NONE', #7271, #21448, #11999, .T. ) ;
#9289 = CARTESIAN_POINT ( 'NONE',  ( 0.000000000000000000, 0.000000000000000000, -0.01377952755905511792 ) ) ;
#9290 = DIRECTION ( 'NONE',  ( 0.000000000000000000, 0.000000000000000000, -1.000000000000000000 ) ) ;
#9291 = PRODUCT_DEFINITION_FORMATION_WITH_SPECIFIED_SOURCE ( 'ANY', '', #14568, .NOT_KNOWN. ) ;
#9292 = EDGE_CURVE ( 'NONE', #12348, #14826, #17508, .T. ) ;
#9293 = CIRCLE ( 'NONE', #20137, 0.09679133858267717494 ) ;
#9294 = DIRECTION ( 'NONE',  ( 0.000000000000000000, 0.000000000000000000, -1.000000000000000000 ) ) ;
#9295 = DIRECTION ( 'NONE',  ( -1.000000000000000000, 0.000000000000000000, 0.000000000000000000 ) ) ;
#9296 = DIRECTION ( 'NONE',  ( 0.000000000000000000, 0.000000000000000000, -1.000000000000000000 ) ) ;
#9297 = DIRECTION ( 'NONE',  ( 0.000000000000000000, 0.000000000000000000, 1.000000000000000000 ) ) ;
#9298 = AXIS2_PLACEMENT_3D ( 'NONE', #4523, #2526, #17375 ) ;
#9299 = ORIENTED_EDGE ( 'NONE', *, *, #13201, .F. ) ;
#9300 = CARTESIAN_POINT ( 'NONE',  ( -0.3149606299212598381, 0.6889763779527560139, 0.000000000000000000 ) ) ;
#9301 = DIRECTION ( 'NONE',  ( 0.000000000000000000, 1.000000000000000000, 0.000000000000000000 ) ) ;
#9302 = DIRECTION ( 'NONE',  ( 0.000000000000000000, -1.000000000000000000, 0.000000000000000000 ) ) ;
#9303 = CARTESIAN_POINT ( 'NONE',  ( 0.3362336590883683307, 0.1141709026133588128, 1.953740157480315043 ) ) ;
#9304 = DIRECTION ( 'NONE',  ( 0.000000000000000000, 0.000000000000000000, -1.000000000000000000 ) ) ;
#9305 = DIRECTION ( 'NONE',  ( 0.000000000000000000, 0.000000000000000000, -1.000000000000000000 ) ) ;
#9306 = CARTESIAN_POINT ( 'NONE',  ( 0.000000000000000000, 0.000000000000000000, 0.1377952755905511861 ) ) ;
#9307 = DIRECTION ( 'NONE',  ( 0.000000000000000000, 0.000000000000000000, 1.000000000000000000 ) ) ;
#9308 = DIRECTION ( 'NONE',  ( 1.000000000000000000, 0.000000000000000000, 0.000000000000000000 ) ) ;
#9309 = VERTEX_POINT ( 'NONE', #5646 ) ;
#9310 = DIRECTION ( 'NONE',  ( 0.000000000000000000, 0.000000000000000000, -1.000000000000000000 ) ) ;
#9311 = CARTESIAN_POINT ( 'NONE',  ( -0.5951974299326810991, -0.1374766578026193065, -0.2478787525163752559 ) ) ;
#9312 = EDGE_CURVE ( 'NONE', #16500, #10335, #2598, .T. ) ;
#9313 = ORIENTED_EDGE ( 'NONE', *, *, #4049, .T. ) ;
#9314 = VERTEX_POINT ( 'NONE', #4587 ) ;
#9315 = EDGE_CURVE ( 'NONE', #17373, #26561, #25853, .T. ) ;
#9316 = LINE ( 'NONE', #2818, #7025 ) ;
#9317 = CARTESIAN_POINT ( 'NONE',  ( 0.5118110236220472231, 6.267877318470705905E-17, 1.914370078775489148 ) ) ;
#9318 = CARTESIAN_POINT ( 'NONE',  ( 0.08600259748440255980, 0.1968503937007873850, -3.597797143241302287 ) ) ;
#9319 = ORIENTED_EDGE ( 'NONE', *, *, #26814, .T. ) ;
#9320 = EDGE_CURVE ( 'NONE', #25431, #25742, #20564, .T. ) ;
#9321 = FACE_OUTER_BOUND ( 'NONE', #9057, .T. ) ;
#9322 = ORIENTED_EDGE ( 'NONE', *, *, #5056, .T. ) ;
#9323 = B_SPLINE_CURVE_WITH_KNOTS ( 'NONE', 3,
 ( #27599, #21518, #5848, #84, #14769, #25327, #10347, #2013, #10197, #10624, #23079, #8514, #27742, #17134, #8242, #16863, #25179, #19105, #18816, #25473, #23224, #6137, #3857, #12617, #3706, #21237, #1875, #10484, #25611, #6266, #25755, #15033, #23646, #4281 ),
 .UNSPECIFIED., .F., .F.,
 ( 4, 2, 2, 2, 2, 2, 2, 2, 2, 2, 2, 2, 2, 2, 2, 2, 4 ),
 ( 0.000000000000000000, 0.03124999999999999306, 0.06249999999999998612, 0.09374999999999997224, 0.1249999999999999722, 0.1562499999999999722, 0.1874999999999999722, 0.2187500000000000000, 0.2500000000000000555, 0.2812500000000000555, 0.3125000000000000555, 0.3437500000000000555, 0.3750000000000000000, 0.4062500000000000000, 0.4375000000000000000, 0.4687500000000000000, 0.5000000000000000000 ),
 .UNSPECIFIED. ) ;
#9324 = CARTESIAN_POINT ( 'NONE',  ( 0.4334967711386992772, -0.2507361369899905879, 0.2574819596263889787 ) ) ;
#9325 = CARTESIAN_POINT ( 'NONE',  ( 0.7845931698711713365, 0.3305999548149256562, -0.3053253099640526602 ) ) ;
#9326 = CARTESIAN_POINT ( 'NONE',  ( 0.000000000000000000, 0.000000000000000000, -0.07578740157480315376 ) ) ;
#9327 = ORIENTED_EDGE ( 'NONE', *, *, #6491, .T. ) ;
#9328 = AXIS2_PLACEMENT_3D ( 'NONE', #23556, #13207, #19716 ) ;
#9329 = CARTESIAN_POINT ( 'NONE',  ( 0.2660793235464269380, 0.2041304421298361926, 1.973425196850393970 ) ) ;
#9330 = CARTESIAN_POINT ( 'NONE',  ( -0.4931105264837953306, 0.08735026989778622852, 0.2574819596263889787 ) ) ;
#9331 = CARTESIAN_POINT ( 'NONE',  ( -0.3382184156749268311, 0.3855916753034290823, -1.550196850393700920 ) ) ;
#9332 = ADVANCED_FACE ( 'NONE', ( #13344, #17586 ), #2467, .T. ) ;
#9333 = CARTESIAN_POINT ( 'NONE',  ( -0.4351030398461813720, -0.1477428134820238381, -1.928289503579156294 ) ) ;
#9334 = DIRECTION ( 'NONE',  ( -1.000000000000000000, 0.000000000000000000, 0.000000000000000000 ) ) ;
#9335 = CARTESIAN_POINT ( 'NONE',  ( -0.4954197419817281123, 0.2442565704126535286, 0.9399606299212598381 ) ) ;
#9336 = CARTESIAN_POINT ( 'NONE',  ( 0.6118597084614586512, 0.1076640027107649555, 0.2574827755769819038 ) ) ;
#9337 = DIRECTION ( 'NONE',  ( 1.000000000000000000, 0.000000000000000000, 0.000000000000000000 ) ) ;
#9338 = DIRECTION ( 'NONE',  ( -1.000000000000000000, 0.000000000000000000, 0.000000000000000000 ) ) ;
#9339 = CARTESIAN_POINT ( 'NONE',  ( -0.2796934465393912106, 0.3645739570812651653, -1.928289503579152742 ) ) ;
#9340 = CARTESIAN_POINT ( 'NONE',  ( 0.1585706980422248169, 0.4669911931914899617, -1.569881889763779625 ) ) ;
#9341 = DIRECTION ( 'NONE',  ( 0.000000000000000000, 0.000000000000000000, -1.000000000000000000 ) ) ;
#9342 = FACE_OUTER_BOUND ( 'NONE', #17613, .T. ) ;
#9343 = CARTESIAN_POINT ( 'NONE',  ( -0.5579526598170320151, -0.3213561723284472094, 0.2359405056215991836 ) ) ;
#9344 = AXIS2_PLACEMENT_3D ( 'NONE', #26564, #7506, #16132 ) ;
#9345 = ADVANCED_FACE ( 'NONE', ( #13205 ), #11222, .T. ) ;
#9346 = EDGE_CURVE ( 'NONE', #4356, #10683, #13656, .T. ) ;
#9347 = AXIS2_PLACEMENT_3D ( 'NONE', #21331, #1829, #2108 ) ;
#9348 = CARTESIAN_POINT ( 'NONE',  ( 0.000000000000000000, 0.000000000000000000, 0.1771653543307086520 ) ) ;
#9349 = STYLED_ITEM ( 'NONE', ( #13806 ), #3076 ) ;
#9350 = PRODUCT_DEFINITION_SHAPE ( 'NONE', 'NONE',  #27908 ) ;
#9351 = DIRECTION ( 'NONE',  ( 0.000000000000000000, 1.000000000000000000, 0.000000000000000000 ) ) ;
#9352 = EDGE_CURVE ( 'NONE', #13928, #858, #6902, .T. ) ;
#9353 = ORIENTED_EDGE ( 'NONE', *, *, #26644, .T. ) ;
#9354 = CARTESIAN_POINT ( 'NONE',  ( 0.1570784101600835037, 0.3184623230425051577, 1.953740157480315043 ) ) ;
#9355 = EDGE_LOOP ( 'NONE', ( #22610, #9386 ) ) ;
#9356 = CARTESIAN_POINT ( 'NONE',  ( 0.3411003281197156900, -0.2991932138496291582, -1.934055118110236338 ) ) ;
#9357 = DIRECTION ( 'NONE',  ( 0.000000000000000000, -0.9850313626640178066, 0.1723752144836030453 ) ) ;
#9358 = CARTESIAN_POINT ( 'NONE',  ( -0.4930758245789425009, 0.08754571829529331217, 0.09685039370078740717 ) ) ;
#9359 = CARTESIAN_POINT ( 'NONE',  ( 0.1517511419330843936, -0.2889986225176974788, -0.3976299462310772248 ) ) ;
#9360 = PLANE ( 'NONE',  #13080 ) ;
#9361 = FACE_BOUND ( 'NONE', #4290, .T. ) ;
#9362 = DIRECTION ( 'NONE',  ( 0.000000000000000000, 1.000000000000000000, 0.000000000000000000 ) ) ;
#9363 = CARTESIAN_POINT ( 'NONE',  ( -0.7874015748031496509, 0.9829781505553011334, -0.2190361720152889935 ) ) ;
#9364 = EDGE_CURVE ( 'NONE', #10805, #25987, #10495, .T. ) ;
#9365 = DIRECTION ( 'NONE',  ( 0.000000000000000000, 0.000000000000000000, -1.000000000000000000 ) ) ;
#9366 = CARTESIAN_POINT ( 'NONE',  ( 8.741913385826771462E-17, -4.420669291338583154E-18, 0.000000000000000000 ) ) ;
#9367 = CARTESIAN_POINT ( 'NONE',  ( 0.2488091035917030791, 0.2836590635674509642, -3.100567304031764948 ) ) ;
#9368 = DIRECTION ( 'NONE',  ( 0.000000000000000000, 1.000000000000000000, 0.000000000000000000 ) ) ;
#9369 = DIRECTION ( 'NONE',  ( -1.000000000000000000, 0.000000000000000000, 0.000000000000000000 ) ) ;
#9370 = ORIENTED_EDGE ( 'NONE', *, *, #10935, .F. ) ;
#9371 = CARTESIAN_POINT ( 'NONE',  ( -0.3535065162672771932, 0.2712027394948494652, -1.934055118110236338 ) ) ;
#9372 = TOROIDAL_SURFACE ( 'NONE', #23856, 0.4232283464566928832, 0.07677165354330708902 ) ;
#9373 = CIRCLE ( 'NONE', #25175, 0.1181102362204718703 ) ;
#9374 = APPLICATION_PROTOCOL_DEFINITION ( 'draft international standard', 'automotive_design', 1998, #22595 ) ;
#9375 = ORIENTED_EDGE ( 'NONE', *, *, #21558, .T. ) ;
#9376 = CARTESIAN_POINT ( 'NONE',  ( 0.3543307086614173040, -0.09842519685039370636, 1.205361022782828035E-17 ) ) ;
#9377 = LINE ( 'NONE', #22536, #20792 ) ;
#9378 = CARTESIAN_POINT ( 'NONE',  ( -0.3382184156732166436, 0.3855916753051391033, 1.747047244094488194 ) ) ;
#9379 = ORIENTED_EDGE ( 'NONE', *, *, #15719, .F. ) ;
#9380 = EDGE_CURVE ( 'NONE', #6360, #6657, #26288, .T. ) ;
#9382 = CARTESIAN_POINT ( 'NONE',  ( -0.3233561589689049609, -0.1867299569291588357, -3.115157480314960647 ) ) ;
#9381 = CARTESIAN_POINT ( 'NONE',  ( 0.000000000000000000, 0.000000000000000000, -0.01377952755905511792 ) ) ;
#9383 = DIRECTION ( 'NONE',  ( 0.000000000000000000, 0.000000000000000000, 1.000000000000000000 ) ) ;
#9384 = CARTESIAN_POINT ( 'NONE',  ( 0.000000000000000000, -0.09092130223458683158, -0.3779527559055118058 ) ) ;
#9385 = EDGE_CURVE ( 'NONE', #19099, #13505, #13802, .T. ) ;
#9386 = ORIENTED_EDGE ( 'NONE', *, *, #7701, .T. ) ;
#9387 = EDGE_LOOP ( 'NONE', ( #16936, #26294, #3835, #589 ) ) ;
#9388 = ORIENTED_EDGE ( 'NONE', *, *, #13013, .F. ) ;
#9389 = ORIENTED_EDGE ( 'NONE', *, *, #16116, .T. ) ;
#9390 = ADVANCED_FACE ( 'NONE', ( #13906, #20117 ), #26465, .T. ) ;
#9391 = AXIS2_PLACEMENT_3D ( 'NONE', #680, #17883, #2774 ) ;
#9392 = DIRECTION ( 'NONE',  ( 1.000000000000000000, 0.000000000000000000, 0.000000000000000000 ) ) ;
#9393 = VERTEX_POINT ( 'NONE', #20400 ) ;
#9394 = ORIENTED_EDGE ( 'NONE', *, *, #992, .F. ) ;
#9395 = ORIENTED_EDGE ( 'NONE', *, *, #25615, .T. ) ;
#9396 = FACE_OUTER_BOUND ( 'NONE', #22391, .T. ) ;
#9397 = SPHERICAL_SURFACE ( 'NONE', #9469, 0.07677362204724409722 ) ;
#9398 = DIRECTION ( 'NONE',  ( 1.000000000000000000, 0.000000000000000000, 0.000000000000000000 ) ) ;
#9399 = DIRECTION ( 'NONE',  ( -1.000000000000000000, 0.000000000000000000, 0.000000000000000000 ) ) ;
#9400 = CIRCLE ( 'NONE', #2203, 0.8163976377952758545 ) ;
#9401 = CARTESIAN_POINT ( 'NONE',  ( 0.5797993700277297435, 0.9434079930944230252, -0.1743634797089741728 ) ) ;
#9402 = CARTESIAN_POINT ( 'NONE',  ( 0.1512183756281842983, -0.2026803072306157250, -0.4450749096211394362 ) ) ;
#9403 = CARTESIAN_POINT ( 'NONE',  ( 0.09586345242798377519, 0.2165354330708661734, -3.246875208232353760 ) ) ;
#9404 = CARTESIAN_POINT ( 'NONE',  ( 0.08759279594700326854, -0.3259357382551449911, 1.973425196850394192 ) ) ;
#9405 = CARTESIAN_POINT ( 'NONE',  ( 0.2341512108694336625, 0.2669480828848126985, 1.953740157480315043 ) ) ;
#9406 = AXIS2_PLACEMENT_3D ( 'NONE', #27219, #16761, #22695 ) ;
#9407 = FACE_OUTER_BOUND ( 'NONE', #19092, .T. ) ;
#9408 = CARTESIAN_POINT ( 'NONE',  ( -0.2313498293151122209, -0.4793777142568558802, 0.1322818204150990051 ) ) ;
#9409 = DIRECTION ( 'NONE',  ( 0.1736481776669309696, 0.9848077530122079093, 0.000000000000000000 ) ) ;
#9410 = ( REPRESENTATION_RELATIONSHIP ('NONE','NONE', #12434, #15008 ) REPRESENTATION_RELATIONSHIP_WITH_TRANSFORMATION ( #23163 )SHAPE_REPRESENTATION_RELATIONSHIP( ) ) ;
#9411 = TOROIDAL_SURFACE ( 'NONE', #8983, 0.4232283464566928832, 0.07677165354330708902 ) ;
#9412 = DIRECTION ( 'NONE',  ( -1.000000000000000000, 0.000000000000000000, 0.000000000000000000 ) ) ;
#9413 = CARTESIAN_POINT ( 'NONE',  ( -0.06957181182498481387, 0.5280699926563169333, 1.747047244094488194 ) ) ;
#9414 = B_SPLINE_CURVE_WITH_KNOTS ( 'NONE', 3,
 ( #6550, #19258, #15326, #17413, #8793, #13166 ),
 .UNSPECIFIED., .F., .F.,
 ( 4, 2, 4 ),
 ( 0.9031406754215579591, 0.9046454396443720514, 0.9061502038671850334 ),
 .UNSPECIFIED. ) ;
#9415 = CARTESIAN_POINT ( 'NONE',  ( -0.07874015747999536796, 0.1968503937007873850, -3.262328874726528660 ) ) ;
#9416 = ORIENTED_EDGE ( 'NONE', *, *, #25752, .T. ) ;
#9417 = COLOUR_RGB ( '', 0.09019608, 0.27058824, 0.51372549) ;
#9418 = CARTESIAN_POINT ( 'NONE',  ( 0.5949363243629232079, -0.1357903337134992172, 0.2362204724409449064 ) ) ;
#9419 = LENGTH_MEASURE_WITH_UNIT ( LENGTH_MEASURE( 0.02539999999999999897 ), #11839 ) ;
#9420 = EDGE_CURVE ( 'NONE', #2922, #20821, #23286, .T. ) ;
#9421 = ORIENTED_EDGE ( 'NONE', *, *, #5472, .F. ) ;
#9422 = CARTESIAN_POINT ( 'NONE',  ( 0.3263749705684267921, -0.1890319631540330891, 0.07637795275590551769 ) ) ;
#9423 = EDGE_LOOP ( 'NONE', ( #11393, #10472 ) ) ;
#9424 = ORIENTED_EDGE ( 'NONE', *, *, #15837, .F. ) ;
#9425 = EDGE_LOOP ( 'NONE', ( #19568, #19081 ) ) ;
#9426 = CARTESIAN_POINT ( 'NONE',  ( 0.3707612262533184766, 0.3252100150720236282, -1.569881889763779625 ) ) ;
#9427 = DIRECTION ( 'NONE',  ( -0.000000000000000000, -1.000000000000000000, -0.000000000000000000 ) ) ;
#9428 = VERTEX_POINT ( 'NONE', #7699 ) ;
#9429 = CARTESIAN_POINT ( 'NONE',  ( -0.5511811023622048555, 0.000000000000000000, 0.9399606299212598381 ) ) ;
#9430 = EDGE_LOOP ( 'NONE', ( #25413, #25440 ) ) ;
#9431 = FACE_BOUND ( 'NONE', #27164, .T. ) ;
#9432 = CIRCLE ( 'NONE', #21181, 0.4724409448465559103 ) ;
#9433 = CARTESIAN_POINT ( 'NONE',  ( 0.000000000000000000, 0.000000000000000000, 1.747047244094488194 ) ) ;
#9434 = ITEM_DEFINED_TRANSFORMATION ( 'NONE', 'NONE', #27411,  #11588 ) ;
#9435 = CARTESIAN_POINT ( 'NONE',  ( -0.09842519685039370636, 0.1673228346456692994, 0.000000000000000000 ) ) ;
#9436 = CARTESIAN_POINT ( 'NONE',  ( -0.0006615832606325197825, 0.6212594902576319411, 0.09685039370078740717 ) ) ;
#9438 = AXIS2_PLACEMENT_3D ( 'NONE', #21199, #8613, #27031 ) ;
#9437 = CARTESIAN_POINT ( 'NONE',  ( -0.4216473064060453635, -0.2427620699883266953, 0.2467937633103768902 ) ) ;
#9439 = FACE_OUTER_BOUND ( 'NONE', #25905, .T. ) ;
#9440 = DIRECTION ( 'NONE',  ( 0.000000000000000000, 0.000000000000000000, 1.000000000000000000 ) ) ;
#9441 = CARTESIAN_POINT ( 'NONE',  ( 0.000000000000000000, -1.533249767903113305E-16, 0.000000000000000000 ) ) ;
#9442 = CARTESIAN_POINT ( 'NONE',  ( -0.02190250779245987017, -0.3346456692913385988, 1.953740157480315043 ) ) ;
#9443 = EDGE_CURVE ( 'NONE', #27816, #5023, #587, .T. ) ;
#9444 = ORIENTED_EDGE ( 'NONE', *, *, #14176, .T. ) ;
#9445 = DIRECTION ( 'NONE',  ( 0.000000000000000000, -1.000000000000000000, 0.000000000000000000 ) ) ;
#9446 = EDGE_CURVE ( 'NONE', #11946, #20489, #12313, .T. ) ;
#9447 = CARTESIAN_POINT ( 'NONE',  ( -0.3123213164510841300, 0.3731274149342653224, 0.09284957166224125369 ) ) ;
#9448 = CARTESIAN_POINT ( 'NONE',  ( -0.1141732283464566844, 0.000000000000000000, 0.000000000000000000 ) ) ;
#9449 = DIRECTION ( 'NONE',  ( 0.000000000000000000, -0.000000000000000000, -1.000000000000000000 ) ) ;
#9450 = CYLINDRICAL_SURFACE ( 'NONE', #9663, 0.5511811023622047445 ) ;
#9451 = CARTESIAN_POINT ( 'NONE',  ( 0.000000000000000000, 0.000000000000000000, 0.07637795275590551769 ) ) ;
#9452 = ADVANCED_FACE ( 'NONE', ( #20546, #20260 ), #22238, .T. ) ;
#9453 = AXIS2_PLACEMENT_3D ( 'NONE', #9289, #25084, #15553 ) ;
#9454 = ORIENTED_EDGE ( 'NONE', *, *, #12692, .F. ) ;
#9455 = CARTESIAN_POINT ( 'NONE',  ( 0.000000000000000000, 0.03937007874015751446, 0.000000000000000000 ) ) ;
#9456 = VECTOR ( 'NONE', #7065, 39.37007874015748143 ) ;
#9457 = EDGE_CURVE ( 'NONE', #16353, #11971, #15481, .T. ) ;
#9458 = EDGE_CURVE ( 'NONE', #21231, #5544, #22380, .T. ) ;
#9459 = ORIENTED_EDGE ( 'NONE', *, *, #14408, .F. ) ;
#9460 = TOROIDAL_SURFACE ( 'NONE', #18012, 0.5915354330708662012, 0.05216535433070866590 ) ;
#9461 = CARTESIAN_POINT ( 'NONE',  ( -0.4858607088160732390, -0.2805118110236220486, 0.07676968503937006694 ) ) ;
#9462 = CARTESIAN_POINT ( 'NONE',  ( -0.3937007874015748254, 1.131889763779527547, 0.000000000000000000 ) ) ;
#9463 = CARTESIAN_POINT ( 'NONE',  ( 0.06048688226684503788, 0.2165354330708661457, -3.626935712454915972 ) ) ;
#9464 = ORIENTED_EDGE ( 'NONE', *, *, #11700, .T. ) ;
#9465 = DIRECTION ( 'NONE',  ( 0.000000000000000000, 0.000000000000000000, 1.000000000000000000 ) ) ;
#9466 = ORIENTED_EDGE ( 'NONE', *, *, #18141, .F. ) ;
#9467 = CARTESIAN_POINT ( 'NONE',  ( 0.6175000359513720394, 0.5702072523746822830, -0.4693776984553832410 ) ) ;
#9468 = CARTESIAN_POINT ( 'NONE',  ( -0.5118110236220472231, -0.03359871295763396104, -1.550196850393701142 ) ) ;
#9469 = AXIS2_PLACEMENT_3D ( 'NONE', #2636, #5316, #5032 ) ;
#9470 = CARTESIAN_POINT ( 'NONE',  ( 0.2988215684303964781, -0.6199272547993208704, 0.1322810039474933141 ) ) ;
#9471 = ORIENTED_EDGE ( 'NONE', *, *, #17530, .T. ) ;
#9472 = VERTEX_POINT ( 'NONE', #9803 ) ;
#9473 = CARTESIAN_POINT ( 'NONE',  ( -0.3346456692913385988, -0.02190250779246036283, 1.973425196850393970 ) ) ;
#9474 = CARTESIAN_POINT ( 'NONE',  ( -0.4669911931914537129, -0.1585706980422384171, -1.550196850393700920 ) ) ;
#9475 = CARTESIAN_POINT ( 'NONE',  ( -0.4816145447621891784, 0.2775852647713620280, 0.9202755905511810219 ) ) ;
#9476 = EDGE_CURVE ( 'NONE', #21655, #6603, #15920, .T. ) ;
#9477 = AXIS2_PLACEMENT_3D ( 'NONE', #27498, #7863, #10105 ) ;
#9478 = CARTESIAN_POINT ( 'NONE',  ( -0.4382482975805320757, -0.3362148458988418187, 0.9202755905511811330 ) ) ;
#9479 = CARTESIAN_POINT ( 'NONE',  ( -0.8725268807032540153, 0.000000000000000000, -0.2362204724409448231 ) ) ;
#9480 = DIRECTION ( 'NONE',  ( -1.000000000000000000, 0.000000000000000000, 0.000000000000000000 ) ) ;
#9481 = CARTESIAN_POINT ( 'NONE',  ( 0.3714653163189441387, 0.06532421472592657430, 0.1992150590373740204 ) ) ;
#9482 = EDGE_CURVE ( 'NONE', #13627, #3934, #27049, .T. ) ;
#9483 = CARTESIAN_POINT ( 'NONE',  ( 0.2466292688015061796, 0.4270824798167727199, -1.569881889763779625 ) ) ;
#9484 = PRESENTATION_STYLE_ASSIGNMENT (( #7524 ) ) ;
#9485 = EDGE_CURVE ( 'NONE', #24074, #720, #16377, .T. ) ;
#9486 = CARTESIAN_POINT ( 'NONE',  ( 0.000000000000000000, 0.6102362204724409711, 0.2362204724409449064 ) ) ;
#9487 = FACE_BOUND ( 'NONE', #27478, .T. ) ;
#9488 = CARTESIAN_POINT ( 'NONE',  ( -0.5491102354219716819, -0.3162573801175062038, 0.1061598535667389875 ) ) ;
#9489 = EDGE_LOOP ( 'NONE', ( #22896, #25049, #12542, #10849 ) ) ;
#9490 = ORIENTED_EDGE ( 'NONE', *, *, #14990, .F. ) ;
#9491 = AXIS2_PLACEMENT_3D ( 'NONE', #10074, #14050, #7542 ) ;
#9492 = CARTESIAN_POINT ( 'NONE',  ( 0.000000000000000000, 0.000000000000000000, -1.550196850393700920 ) ) ;
#9493 = DIRECTION ( 'NONE',  ( 0.000000000000000000, 0.000000000000000000, 1.000000000000000000 ) ) ;
#9494 = VERTEX_POINT ( 'NONE', #5575 ) ;
#9495 = CARTESIAN_POINT ( 'NONE',  ( -0.09193072188187405291, 0.3429848536918321256, 1.953740157480315043 ) ) ;
#9496 = VERTEX_POINT ( 'NONE', #11504 ) ;
#9497 = AXIS2_PLACEMENT_3D ( 'NONE', #27644, #8288, #10530 ) ;
#9498 = CARTESIAN_POINT ( 'NONE',  ( 0.1458850421962362143, -0.4296318976989931815, -1.934055118110236338 ) ) ;
#9499 = CARTESIAN_POINT ( 'NONE',  ( 0.4067073728345488304, -0.2341441294389854655, 0.07637795275590551769 ) ) ;
#9500 = CARTESIAN_POINT ( 'NONE',  ( 0.3713448905834433322, 0.06600512665679410251, 0.07637795275590551769 ) ) ;
#9501 = CARTESIAN_POINT ( 'NONE',  ( -0.07874015748031495954, 0.04546065111729338803, -0.4724409448818898127 ) ) ;
#9502 = CARTESIAN_POINT ( 'NONE',  ( 0.003937007874015826907, -4.393043307086613241E-18, 0.000000000000000000 ) ) ;
#9503 = DIRECTION ( 'NONE',  ( 0.000000000000000000, 0.000000000000000000, 1.000000000000000000 ) ) ;
#9504 = DIRECTION ( 'NONE',  ( 1.000000000000000000, 5.737213000000000442E-16, 0.000000000000000000 ) ) ;
#9505 = DIRECTION ( 'NONE',  ( 0.000000000000000000, 1.000000000000000000, 0.000000000000000000 ) ) ;
#9506 = CARTESIAN_POINT ( 'NONE',  ( 0.3740848232703729015, -0.04928467685644277729, -3.100567304031765392 ) ) ;
#9507 = FACE_BOUND ( 'NONE', #14650, .T. ) ;
#9508 = B_SPLINE_CURVE_WITH_KNOTS ( 'NONE', 3,
 ( #15122, #8871, #12836, #12693, #420, #19336 ),
 .UNSPECIFIED., .F., .F.,
 ( 4, 2, 4 ),
 ( 0.000000000000000000, 0.2500000000000001665, 0.5000000000000000000 ),
 .UNSPECIFIED. ) ;
#9509 = ORIENTED_EDGE ( 'NONE', *, *, #5628, .F. ) ;
#9510 = CARTESIAN_POINT ( 'NONE',  ( -0.4218945342797526532, -0.1432577568504610210, -1.934055118110236338 ) ) ;
#9511 = ADVANCED_FACE ( 'NONE', ( #14202 ), #17283, .T. ) ;
#9512 = CONICAL_SURFACE ( 'NONE', #26229, 0.4863540308881693086, 1.365720138124999927 ) ;
#9513 = ADVANCED_FACE ( 'NONE', ( #25487, #27611 ), #8396, .T. ) ;
#9514 = APPLICATION_PROTOCOL_DEFINITION ( 'draft international standard', 'automotive_design', 1998, #3649 ) ;
#9515 = CIRCLE ( 'NONE', #22156, 0.6212598425196850238 ) ;
#9516 = VECTOR ( 'NONE', #8406, 39.37007874015748854 ) ;
#9517 = ORIENTED_EDGE ( 'NONE', *, *, #5794, .F. ) ;
#9518 = VERTEX_POINT ( 'NONE', #21389 ) ;
#9519 = CARTESIAN_POINT ( 'NONE',  ( -0.4101012214746874163, -0.9083388034714960924, -0.1356156739343915285 ) ) ;
#9520 = DIRECTION ( 'NONE',  ( 1.000000000000000000, 0.000000000000000000, 0.000000000000000000 ) ) ;
#9521 = FACE_OUTER_BOUND ( 'NONE', #23452, .T. ) ;
#9522 = CARTESIAN_POINT ( 'NONE',  ( 0.4600326175560556230, -0.2268096725222457644, 1.766732283464566899 ) ) ;
#9523 = CARTESIAN_POINT ( 'NONE',  ( 0.3529960615022520454, 0.06172929298841274559, 0.1805249803415999998 ) ) ;
#9524 = ORIENTED_EDGE ( 'NONE', *, *, #10981, .F. ) ;
#9525 = CARTESIAN_POINT ( 'NONE',  ( 0.2836590635674519634, 0.2488091035917033567, -3.100567304031761395 ) ) ;
#9526 = ORIENTED_EDGE ( 'NONE', *, *, #5522, .T. ) ;
#9527 = CARTESIAN_POINT ( 'NONE',  ( -0.4585215200179055817, 0.000000000000000000, -1.928289503579156516 ) ) ;
#9528 = CARTESIAN_POINT ( 'NONE',  ( -0.2070393714800602414, -0.09900904606225019444, 0.07874015748031495954 ) ) ;
#9529 = ORIENTED_EDGE ( 'NONE', *, *, #18476, .F. ) ;
#9530 = EDGE_LOOP ( 'NONE', ( #21260, #6337, #21119, #291 ) ) ;
#9531 = VECTOR ( 'NONE', #8218, 39.37007874015748143 ) ;
#9532 = CARTESIAN_POINT ( 'NONE',  ( -0.3458583018457046521, -0.7501511824813903440, -0.7295201136257942753 ) ) ;
#9533 = CARTESIAN_POINT ( 'NONE',  ( -0.5241918773311228241, 0.000000000000000000, -0.2204724409448818867 ) ) ;
#9534 = ORIENTED_EDGE ( 'NONE', *, *, #23489, .F. ) ;
#9535 = CARTESIAN_POINT ( 'NONE',  ( 0.4446020952038907681, -0.02909913904662010317, -1.934055118110236338 ) ) ;
#9536 = EDGE_LOOP ( 'NONE', ( #23774, #17213, #27563 ) ) ;
#9537 = DIRECTION ( 'NONE',  ( 0.9790454724845839563, 0.2036417511401769909, -2.493892000000000165E-17 ) ) ;
#9538 = CARTESIAN_POINT ( 'NONE',  ( 0.04841158226352236527, 0.1968503937007874127, -3.611176134491095091 ) ) ;
#9539 = CIRCLE ( 'NONE', #9081, 0.1299212598425196763 ) ;
#9540 = B_SPLINE_CURVE_WITH_KNOTS ( 'NONE', 3,
 ( #6977, #15463, #21951, #24062, #22075, #4696, #13591, #5108, #26580, #13322 ),
 .UNSPECIFIED., .F., .F.,
 ( 4, 2, 2, 2, 4 ),
 ( 0.000000000000000000, 0.2500000000000000000, 0.5000000000000000000, 0.7500000000000000000, 1.000000000000000000 ),
 .UNSPECIFIED. ) ;
#9541 = CARTESIAN_POINT ( 'NONE',  ( -0.3204319178471763951, -0.6672004808837513901, 0.2562996996000485028 ) ) ;
#9542 = CARTESIAN_POINT ( 'NONE',  ( 0.3346456692913385988, 0.04380501567505457050, 1.973425196850394192 ) ) ;
#9543 = DIRECTION ( 'NONE',  ( -1.000000000000000000, 0.000000000000000000, 0.000000000000000000 ) ) ;
#9544 = ADVANCED_FACE ( 'NONE', ( #14487 ), #23138, .T. ) ;
#9545 = DIRECTION ( 'NONE',  ( 0.000000000000000000, 0.000000000000000000, -1.000000000000000000 ) ) ;
#9546 = CARTESIAN_POINT ( 'NONE',  ( -0.4065144339881338054, -0.2344790234878023627, 0.1992150590373740204 ) ) ;
#9547 = DIRECTION ( 'NONE',  ( -0.000000000000000000, -0.000000000000000000, -1.000000000000000000 ) ) ;
#9548 = CARTESIAN_POINT ( 'NONE',  ( -0.3520466617656974884, -0.04638120790932648285, 1.953740157480315043 ) ) ;
#9549 = EDGE_CURVE ( 'NONE', #10943, #11887, #2367, .T. ) ;
#9550 = AXIS2_PLACEMENT_3D ( 'NONE', #1527, #9860, #8039 ) ;
#9551 = ORIENTED_EDGE ( 'NONE', *, *, #22970, .T. ) ;
#9552 = CARTESIAN_POINT ( 'NONE',  ( 0.4898768902087983768, 0.000000000000000000, -0.2362204724409449064 ) ) ;
#9553 = CARTESIAN_POINT ( 'NONE',  ( -0.4685039370078740717, 0.000000000000000000, -0.006889763779527558960 ) ) ;
#9554 = CARTESIAN_POINT ( 'NONE',  ( -0.01453548245982153216, -0.08252923752360777354, -0.4702630791244896136 ) ) ;
#9555 = DIRECTION ( 'NONE',  ( 0.000000000000000000, 1.000000000000000000, 0.000000000000000000 ) ) ;
#9556 = CARTESIAN_POINT ( 'NONE',  ( -0.4004221243553298115, -0.3512268162760094348, 1.747047244094488194 ) ) ;
#9557 = LINE ( 'NONE', #7450, #26195 ) ;
#9558 = AXIS2_PLACEMENT_3D ( 'NONE', #8700, #6041, #2202 ) ;
#9559 = CARTESIAN_POINT ( 'NONE',  ( 0.000000000000000000, 0.000000000000000000, 0.5905511811023621549 ) ) ;
#9560 = EDGE_LOOP ( 'NONE', ( #16017, #9464, #14779, #25368, #20740, #15992 ) ) ;
#9561 = CARTESIAN_POINT ( 'NONE',  ( 0.2195865873864355222, -0.6052790189103738339, 0.2359405056189624594 ) ) ;
#9562 = DIRECTION ( 'NONE',  ( 1.000000000000000000, 0.000000000000000000, 0.000000000000000000 ) ) ;
#9563 = EDGE_CURVE ( 'NONE', #4513, #11373, #7354, .T. ) ;
#9564 = ORIENTED_EDGE ( 'NONE', *, *, #18039, .F. ) ;
#9565 = CARTESIAN_POINT ( 'NONE',  ( 0.03220957031753916844, -0.4921259842519686289, -1.569881889763779625 ) ) ;
#9566 = EDGE_LOOP ( 'NONE', ( #22929, #1313 ) ) ;
#9567 = CARTESIAN_POINT ( 'NONE',  ( -0.5131133041953912510, 0.2529800193559492705, 0.9399606299212598381 ) ) ;
#9568 = ORIENTED_EDGE ( 'NONE', *, *, #20277, .F. ) ;
#9569 = VERTEX_POINT ( 'NONE', #16878 ) ;
#9570 = FACE_OUTER_BOUND ( 'NONE', #13886, .T. ) ;
#9571 = CARTESIAN_POINT ( 'NONE',  ( -0.1968503937007874127, -5.802129921259842692E-18, 0.000000000000000000 ) ) ;
#9572 = AXIS2_PLACEMENT_3D ( 'NONE', #14638, #12763, #17010 ) ;
#9573 = ITEM_DEFINED_TRANSFORMATION ( 'NONE', 'NONE', #2584,  #11588 ) ;
#9574 = PLANE ( 'NONE',  #13535 ) ;
#9575 = B_SPLINE_CURVE_WITH_KNOTS ( 'NONE', 3,
 ( #24680, #13966, #5492, #1118, #26962, #14103 ),
 .UNSPECIFIED., .F., .F.,
 ( 4, 2, 4 ),
 ( 1.217380381967464009, 1.219305002860850085, 1.221229623754233939 ),
 .UNSPECIFIED. ) ;
#9576 = DIRECTION ( 'NONE',  ( 1.000000000000000000, 0.000000000000000000, 0.000000000000000000 ) ) ;
#9577 = CARTESIAN_POINT ( 'NONE',  ( 3.168943700787402105E-16, -0.6299212598425196763, 0.000000000000000000 ) ) ;
#9578 = CARTESIAN_POINT ( 'NONE',  ( -0.4620947063919622066, 0.08187111969652559329, 0.1992142434433716580 ) ) ;
#9579 = DIRECTION ( 'NONE',  ( 0.000000000000000000, 1.000000000000000000, 0.000000000000000000 ) ) ;
#9580 = CIRCLE ( 'NONE', #9140, 0.1298643763538141760 ) ;
#9581 = DIRECTION ( 'NONE',  ( 0.000000000000000000, 0.000000000000000000, -1.000000000000000000 ) ) ;
#9582 = CYLINDRICAL_SURFACE ( 'NONE', #21807, 0.8267716535433071723 ) ;
#9583 = CARTESIAN_POINT ( 'NONE',  ( 0.3543307086614173596, 0.000000000000000000, 1.953740157480315043 ) ) ;
#9584 = EDGE_CURVE ( 'NONE', #13641, #25766, #23613, .T. ) ;
#9585 = UNCERTAINTY_MEASURE_WITH_UNIT (LENGTH_MEASURE( 1.000000000000000082E-05 ), #14261, 'distance_accuracy_value', 'NONE') ;
#9586 = EDGE_LOOP ( 'NONE', ( #22344, #9756, #14033, #23346 ) ) ;
#9587 = DIRECTION ( 'NONE',  ( 0.000000000000000000, 1.000000000000000000, 0.000000000000000000 ) ) ;
#9588 = CARTESIAN_POINT ( 'NONE',  ( 0.000000000000000000, 0.000000000000000000, -0.01377952755905511792 ) ) ;
#9589 = CARTESIAN_POINT ( 'NONE',  ( -0.6142148233928379497, -0.1505053300589599685, 0.2274168496461167199 ) ) ;
#9590 = DIRECTION ( 'NONE',  ( 0.000000000000000000, 0.000000000000000000, 1.000000000000000000 ) ) ;
#9591 = PRODUCT_DEFINITION_SHAPE ( 'NONE', 'NONE',  #27907 ) ;
#9592 = DIRECTION ( 'NONE',  ( 0.000000000000000000, 0.000000000000000000, -1.000000000000000000 ) ) ;
#9593 = CARTESIAN_POINT ( 'NONE',  ( 0.7874015748031496509, -3.035194737559056185E-06, -1.475314960619023674 ) ) ;
#9594 = CIRCLE ( 'NONE', #20437, 0.7283464566929134243 ) ;
#9595 = CARTESIAN_POINT ( 'NONE',  ( 0.1522836969735573143, -0.4909267390297480382, -0.05591742528025173131 ) ) ;
#9596 = AXIS2_PLACEMENT_3D ( 'NONE', #20645, #23354, #1298 ) ;
#9597 = VERTEX_POINT ( 'NONE', #9941 ) ;
#9598 = AXIS2_PLACEMENT_3D ( 'NONE', #2624, #4488, #17341 ) ;
#9599 = ORIENTED_EDGE ( 'NONE', *, *, #17818, .F. ) ;
#9600 = AXIS2_PLACEMENT_3D ( 'NONE', #23174, #21468, #3951 ) ;
#9601 = DIRECTION ( 'NONE',  ( 1.147443000000000016E-15, 1.000000000000000000, -1.224646799147353207E-16 ) ) ;
#9602 = CARTESIAN_POINT ( 'NONE',  ( 0.2256712916308122319, 0.000000000000000000, -4.330708661396418080 ) ) ;
#9603 = VECTOR ( 'NONE', #7035, 39.37007874015748143 ) ;
#9604 = CARTESIAN_POINT ( 'NONE',  ( 0.02576258753917241504, 0.1968503937008544147, -3.644091798679202299 ) ) ;
#9605 = EDGE_LOOP ( 'NONE', ( #10989, #10775 ) ) ;
#9606 = CYLINDRICAL_SURFACE ( 'NONE', #8142, 0.7539370078740157410 ) ;
#9607 = ORIENTED_EDGE ( 'NONE', *, *, #8917, .T. ) ;
#9608 = EDGE_CURVE ( 'NONE', #1867, #8441, #6277, .T. ) ;
#9609 = ( CONVERSION_BASED_UNIT ( 'INCH', #6823 ) LENGTH_UNIT ( ) NAMED_UNIT ( #7787 ) ) ;
#9610 = CARTESIAN_POINT ( 'NONE',  ( 0.7845931698711713365, 0.3318803385907665437, -0.3024313949403425461 ) ) ;
#9611 = B_SPLINE_CURVE_WITH_KNOTS ( 'NONE', 3,
 ( #9855, #12117, #18747, #24967 ),
 .UNSPECIFIED., .F., .F.,
 ( 4, 4 ),
 ( 0.000000000000000000, 1.000000000000000000 ),
 .UNSPECIFIED. ) ;
#9612 = AXIS2_PLACEMENT_3D ( 'NONE', #24329, #4977, #19439 ) ;
#9613 = CIRCLE ( 'NONE', #1006, 0.07677362204724411110 ) ;
#9614 = CYLINDRICAL_SURFACE ( 'NONE', #15941, 0.4685039370078740717 ) ;
#9615 = CARTESIAN_POINT ( 'NONE',  ( 0.6889763779527560139, 8.437527159479796553E-17, -0.01377952755905511792 ) ) ;
#9616 = ADVANCED_FACE ( 'NONE', ( #4017 ), #6151, .F. ) ;
#9617 = EDGE_LOOP ( 'NONE', ( #13184, #26695, #14076, #18493 ) ) ;
#9618 = ORIENTED_EDGE ( 'NONE', *, *, #11461, .T. ) ;
#9619 = CARTESIAN_POINT ( 'NONE',  ( 0.09842519685039358146, 0.2991866959364303802, -3.548228346456693050 ) ) ;
#9620 = CARTESIAN_POINT ( 'NONE',  ( -0.4921259842519685179, 0.000000000000000000, -1.550196850393700920 ) ) ;
#9621 = CARTESIAN_POINT ( 'NONE',  ( -0.3714054139060130044, 0.06566393819133267695, 0.07637549214372835182 ) ) ;
#9622 = VECTOR ( 'NONE', #20864, 39.37007874015748143 ) ;
#9623 = CARTESIAN_POINT ( 'NONE',  ( 0.4152525734086276454, 0.3642352168757554964, 0.9202755905511811330 ) ) ;
#9624 = DIRECTION ( 'NONE',  ( -1.000000000000000000, 0.000000000000000000, 0.000000000000000000 ) ) ;
#9625 = VECTOR ( 'NONE', #27184, 39.37007874015748143 ) ;
#9626 = DIRECTION ( 'NONE',  ( 0.000000000000000000, 0.000000000000000000, 1.000000000000000000 ) ) ;
#9627 = CARTESIAN_POINT ( 'NONE',  ( -0.2315507648392299000, -0.4792806379917101678, 0.3401574803149606252 ) ) ;
#9628 = ( REPRESENTATION_RELATIONSHIP ('NONE','NONE', #12434, #19852 ) REPRESENTATION_RELATIONSHIP_WITH_TRANSFORMATION ( #12837 )SHAPE_REPRESENTATION_RELATIONSHIP( ) ) ;
#9629 = CARTESIAN_POINT ( 'NONE',  ( 0.000000000000000000, 0.000000000000000000, -0.07578740157480315376 ) ) ;
#9630 = DIRECTION ( 'NONE',  ( 0.000000000000000000, 1.000000000000000000, 0.000000000000000000 ) ) ;
#9631 = CARTESIAN_POINT ( 'NONE',  ( 0.1710938124795997883, -0.4706537664821763833, 0.2574827755769819038 ) ) ;
#9632 = DIRECTION ( 'NONE',  ( 0.8660254037844385966, -0.5000000000000003331, 0.000000000000000000 ) ) ;
#9633 = CARTESIAN_POINT ( 'NONE',  ( 0.4245040230929275626, 1.106753849019775471, -0.3897420188601015689 ) ) ;
#9634 = CIRCLE ( 'NONE', #20031, 0.6889763779527560139 ) ;
#9635 = EDGE_LOOP ( 'NONE', ( #20274, #21132 ) ) ;
#9636 = CARTESIAN_POINT ( 'NONE',  ( 8.741913385826771462E-17, -4.420669291338583154E-18, 0.000000000000000000 ) ) ;
#9637 = CARTESIAN_POINT ( 'NONE',  ( 0.000000000000000000, 0.000000000000000000, -4.291338582656260670 ) ) ;
#9638 = CIRCLE ( 'NONE', #26851, 1.377952755905512472 ) ;
#9639 = ORIENTED_EDGE ( 'NONE', *, *, #16301, .T. ) ;
#9640 = CARTESIAN_POINT ( 'NONE',  ( 6.557635703933409897E-17, 0.3771653543307084688, 0.07637549214372833795 ) ) ;
#9641 = CARTESIAN_POINT ( 'NONE',  ( -0.1181102362204724532, 0.000000000000000000, 0.000000000000000000 ) ) ;
#9642 = ORIENTED_EDGE ( 'NONE', *, *, #4507, .T. ) ;
#9643 = EDGE_LOOP ( 'NONE', ( #8449, #6690, #6206, #22522 ) ) ;
#9644 = EDGE_CURVE ( 'NONE', #19740, #24937, #13153, .T. ) ;
#9645 = CIRCLE ( 'NONE', #17325, 0.1181102362204720091 ) ;
#9646 = CARTESIAN_POINT ( 'NONE',  ( 0.4296318976989619842, -0.1458850421962461508, -1.934055118110236338 ) ) ;
#9647 = B_SPLINE_CURVE_WITH_KNOTS ( 'NONE', 3,
 ( #27372, #8926, #15036, #10917, #4286, #2690 ),
 .UNSPECIFIED., .F., .F.,
 ( 4, 2, 4 ),
 ( 0.000000000000000000, 0.5000000000000000000, 1.000000000000000000 ),
 .UNSPECIFIED. ) ;
#9648 = LINE ( 'NONE', #24476, #14411 ) ;
#9649 = CARTESIAN_POINT ( 'NONE',  ( -0.1610509776512594748, -0.4407912692718567449, 0.1992125984251968684 ) ) ;
#9650 = LINE ( 'NONE', #16436, #14639 ) ;
#9651 = AXIS2_PLACEMENT_3D ( 'NONE', #2102, #12423, #10715 ) ;
#9652 = DIRECTION ( 'NONE',  ( 1.000000000000000000, 0.000000000000000000, 0.000000000000000000 ) ) ;
#9653 = ORIENTED_EDGE ( 'NONE', *, *, #7386, .F. ) ;
#9654 = DIRECTION ( 'NONE',  ( 0.000000000000000000, 0.000000000000000000, 1.000000000000000000 ) ) ;
#9655 = EDGE_CURVE ( 'NONE', #21760, #13891, #21780, .T. ) ;
#9656 = ORIENTED_EDGE ( 'NONE', *, *, #21085, .F. ) ;
#9657 = DIRECTION ( 'NONE',  ( 0.000000000000000000, 0.000000000000000000, -1.000000000000000000 ) ) ;
#9658 = ORIENTED_EDGE ( 'NONE', *, *, #11931, .T. ) ;
#9659 = CARTESIAN_POINT ( 'NONE',  ( -0.2488091035917009419, 0.2836590635674538508, -3.100567304031763172 ) ) ;
#9660 = EDGE_CURVE ( 'NONE', #21106, #16322, #21249, .T. ) ;
#9661 = DIRECTION ( 'NONE',  ( 0.000000000000000000, 0.000000000000000000, 1.000000000000000000 ) ) ;
#9662 = B_SPLINE_CURVE_WITH_KNOTS ( 'NONE', 3,
 ( #7490, #25250, #16117, #12396, #23144, #10410, #14687, #21155, #16636, #27524 ),
 .UNSPECIFIED., .F., .F.,
 ( 4, 2, 2, 2, 4 ),
 ( 0.000000000000000000, 0.2500000000000001110, 0.5000000000000002220, 0.7500000000000003331, 1.000000000000000000 ),
 .UNSPECIFIED. ) ;
#9663 = AXIS2_PLACEMENT_3D ( 'NONE', #18050, #7350, #9174 ) ;
#9664 = PRODUCT_DEFINITION_CONTEXT ( 'detailed design', #22258, 'design' ) ;
#9665 = VERTEX_POINT ( 'NONE', #1607 ) ;
#9666 = CARTESIAN_POINT ( 'NONE',  ( 0.3535065162672720307, 0.2712027394948698378, -1.934055118110236338 ) ) ;
#9667 = CARTESIAN_POINT ( 'NONE',  ( -0.4438564651657478377, 0.1188866373884873845, -1.928289503579152742 ) ) ;
#9668 = AXIS2_PLACEMENT_3D ( 'NONE', #1003, #13849, #27133 ) ;
#9669 = ( CONVERSION_BASED_UNIT ( 'INCH', #9948 ) LENGTH_UNIT ( ) NAMED_UNIT ( #2029 ) ) ;
#9670 = CIRCLE ( 'NONE', #27748, 0.01181102362204724393 ) ;
#9671 = CARTESIAN_POINT ( 'NONE',  ( -0.3681444341728476455, -0.6850021075794429093, -0.6051803271985433108 ) ) ;
#9672 = FACE_OUTER_BOUND ( 'NONE', #25485, .T. ) ;
#9673 = CARTESIAN_POINT ( 'NONE',  ( 0.4441657790107856330, -0.2564944395515579845, 1.766732283464566899 ) ) ;
#9674 = ORIENTED_EDGE ( 'NONE', *, *, #26682, .T. ) ;
#9675 = FILL_AREA_STYLE_COLOUR ( '', #17021 ) ;
#9676 = ORIENTED_EDGE ( 'NONE', *, *, #13598, .T. ) ;
#9677 = CARTESIAN_POINT ( 'NONE',  ( -0.2993674444872274076, -0.2296683860596782090, -3.100567304031764060 ) ) ;
#9678 = VERTEX_POINT ( 'NONE', #10496 ) ;
#9679 = FACE_OUTER_BOUND ( 'NONE', #1946, .T. ) ;
#9680 = CARTESIAN_POINT ( 'NONE',  ( -0.2602238532265429005, 0.000000000000000000, -0.2362204724409449064 ) ) ;
#9681 = VECTOR ( 'NONE', #12940, 39.37007874015748143 ) ;
#9682 = ORIENTED_EDGE ( 'NONE', *, *, #11287, .F. ) ;
#9683 = EDGE_CURVE ( 'NONE', #8364, #4142, #13196, .T. ) ;
#9684 = CARTESIAN_POINT ( 'NONE',  ( 0.000000000000000000, 0.000000000000000000, -0.2755905511811023723 ) ) ;
#9685 = DIRECTION ( 'NONE',  ( -1.000000000000000000, 0.000000000000000000, 0.000000000000000000 ) ) ;
#9686 = ORIENTED_EDGE ( 'NONE', *, *, #13053, .F. ) ;
#9687 = CARTESIAN_POINT ( 'NONE',  ( -0.1432577568504724008, -0.4218945342797531528, -1.934055118110236338 ) ) ;
#9688 = EDGE_LOOP ( 'NONE', ( #6476, #406, #24034, #9197 ) ) ;
#9689 = EDGE_LOOP ( 'NONE', ( #16489, #870, #20492, #16523 ) ) ;
#9690 = FACE_BOUND ( 'NONE', #13395, .T. ) ;
#9691 = DIRECTION ( 'NONE',  ( 0.000000000000000000, 0.000000000000000000, -1.000000000000000000 ) ) ;
#9692 = ADVANCED_FACE ( 'NONE', ( #16445 ), #15043, .F. ) ;
#9693 = CONICAL_SURFACE ( 'NONE', #2036, 0.4863540308881693086, 1.365720138124999927 ) ;
#9694 = CARTESIAN_POINT ( 'NONE',  ( 0.4898768902087983768, -4.281484251968504304E-16, 0.2362204724409449064 ) ) ;
#9695 = CARTESIAN_POINT ( 'NONE',  ( 0.000000000000000000, 0.4232283464566928832, 0.1377952755905511861 ) ) ;
#9696 = LINE ( 'NONE', #18296, #11621 ) ;
#9697 = CARTESIAN_POINT ( 'NONE',  ( 0.5485639935000311551, 0.9796862869722393619, -0.2151333194223323253 ) ) ;
#9698 = ( BOUNDED_CURVE ( )  B_SPLINE_CURVE ( 2, ( #26159, #8918, #24037 ),
 .UNSPECIFIED., .F., .T. ) 
 B_SPLINE_CURVE_WITH_KNOTS ( ( 3, 3 ),
 ( 0.1168436138077914160, 0.2336872276155829709 ),
 .UNSPECIFIED. ) 
 CURVE ( )  GEOMETRIC_REPRESENTATION_ITEM ( )  RATIONAL_B_SPLINE_CURVE ( ( 1.077350269189623067, 1.077350269189623067, 1.000000000000000000 ) ) 
 REPRESENTATION_ITEM ( '' )  ) ;
#9699 = DIRECTION ( 'NONE',  ( 1.000000000000000000, 0.000000000000000000, 0.000000000000000000 ) ) ;
#9700 = CARTESIAN_POINT ( 'NONE',  ( -0.3346456692913385988, 2.134256245050205639E-17, 1.973425196850393970 ) ) ;
#9701 = CARTESIAN_POINT ( 'NONE',  ( 0.02319089060378217229, -0.3543307086614173596, 1.953740157480315043 ) ) ;
#9702 = CIRCLE ( 'NONE', #273, 0.3722026523000413478 ) ;
#9703 = ADVANCED_FACE ( 'NONE', ( #16580 ), #14339, .T. ) ;
#9704 = ORIENTED_EDGE ( 'NONE', *, *, #235, .F. ) ;
#9705 = LINE ( 'NONE', #13955, #10999 ) ;
#9706 = CARTESIAN_POINT ( 'NONE',  ( -0.5511811023622047445, 6.750021727583836750E-17, 0.01181102362204724393 ) ) ;
#9707 = DIRECTION ( 'NONE',  ( 0.000000000000000000, 0.000000000000000000, 1.000000000000000000 ) ) ;
#9708 = CARTESIAN_POINT ( 'NONE',  ( -0.03532354024591771724, -0.6299212598425196763, 0.000000000000000000 ) ) ;
#9709 = DIRECTION ( 'NONE',  ( 0.9749279121818236193, -0.2225209339563147815, 0.000000000000000000 ) ) ;
#9710 = CARTESIAN_POINT ( 'NONE',  ( 0.4004221243553300891, 0.3512268162760394108, 1.747047244094488194 ) ) ;
#9711 = DIRECTION ( 'NONE',  ( 0.000000000000000000, 0.000000000000000000, 1.000000000000000000 ) ) ;
#9712 = CARTESIAN_POINT ( 'NONE',  ( 0.3121994997598087074, 0.4069448477555728250, 1.747047244094488194 ) ) ;
#9713 = AXIS2_PLACEMENT_3D ( 'NONE', #22939, #1455, #25181 ) ;
#9714 = VERTEX_POINT ( 'NONE', #18826 ) ;
#9715 = CARTESIAN_POINT ( 'NONE',  ( -0.2180698645301862859, 0.2842490391651604775, -3.115157480314960647 ) ) ;
#9716 = ORIENTED_EDGE ( 'NONE', *, *, #2318, .T. ) ;
#9717 = CIRCLE ( 'NONE', #25499, 0.1003956692913385712 ) ;
#9718 = DIRECTION ( 'NONE',  ( 0.000000000000000000, 0.000000000000000000, 1.000000000000000000 ) ) ;
#9719 = CARTESIAN_POINT ( 'NONE',  ( 0.2997912780622379869, -0.1736589463928938648, 0.1276989850557191386 ) ) ;
#9720 = VERTEX_POINT ( 'NONE', #23237 ) ;
#9721 = ORIENTED_EDGE ( 'NONE', *, *, #13412, .F. ) ;
#9722 = EDGE_CURVE ( 'NONE', #21448, #1673, #12486, .T. ) ;
#9723 = CARTESIAN_POINT ( 'NONE',  ( 0.1275996891957757451, -0.4763861460130329184, -1.569881889763779625 ) ) ;
#9724 = ADVANCED_FACE ( 'NONE', ( #23659 ), #13314, .T. ) ;
#9725 = ORIENTED_EDGE ( 'NONE', *, *, #666, .F. ) ;
#9726 = ORIENTED_EDGE ( 'NONE', *, *, #19797, .T. ) ;
#9727 = ADVANCED_FACE ( 'NONE', ( #17145 ), #8659, .F. ) ;
#9728 = CIRCLE ( 'NONE', #13337, 0.6881889763779527325 ) ;
#9729 = ITEM_DEFINED_TRANSFORMATION ( 'NONE', 'NONE', #3012,  #11588 ) ;
#9730 = FACE_OUTER_BOUND ( 'NONE', #15, .T. ) ;
#9731 = DIRECTION ( 'NONE',  ( 0.000000000000000000, 0.000000000000000000, -1.000000000000000000 ) ) ;
#9732 = CARTESIAN_POINT ( 'NONE',  ( -9.506830708661417994E-16, -0.8267716535433071723, 0.000000000000000000 ) ) ;
#9733 = CARTESIAN_POINT ( 'NONE',  ( -0.6995386212070490162, 0.8547296533447173994, -0.08348329912257269891 ) ) ;
#9734 = CARTESIAN_POINT ( 'NONE',  ( 0.000000000000000000, 0.000000000000000000, 0.2362204724409449064 ) ) ;
#9735 = EDGE_CURVE ( 'NONE', #3239, #5530, #17284, .T. ) ;
#9736 = CARTESIAN_POINT ( 'NONE',  ( -0.7874015748031496509, 0.9829781505553011334, -0.2190361720152889935 ) ) ;
#9737 = CONICAL_SURFACE ( 'NONE', #5676, 0.08876456692913387014, 0.7853981624999977207 ) ;
#9738 = CARTESIAN_POINT ( 'NONE',  ( -0.1482986320106521871, -0.3007905576423956506, 1.953740157480315043 ) ) ;
#9739 = EDGE_CURVE ( 'NONE', #25182, #25584, #14606, .T. ) ;
#9740 = ORIENTED_EDGE ( 'NONE', *, *, #13812, .F. ) ;
#9741 = CYLINDRICAL_SURFACE ( 'NONE', #23621, 0.06200787401574775481 ) ;
#9742 = CARTESIAN_POINT ( 'NONE',  ( 0.07874015748031495954, -0.04546065111729338803, -0.4724409448818898127 ) ) ;
#9743 = CARTESIAN_POINT ( 'NONE',  ( -0.3031496062992123375, 0.000000000000000000, -0.02362204724409448786 ) ) ;
#9744 = PLANE ( 'NONE',  #3807 ) ;
#9745 = CARTESIAN_POINT ( 'NONE',  ( -0.4173228346456693272, 5.110730736599190647E-17, 0.02362204724409448786 ) ) ;
#9746 = CARTESIAN_POINT ( 'NONE',  ( -0.4713455951393992760, -0.1082342125223313134, 0.2008762816256353667 ) ) ;
#9747 = FACE_BOUND ( 'NONE', #627, .T. ) ;
#9748 = ORIENTED_EDGE ( 'NONE', *, *, #20283, .T. ) ;
#9749 = EDGE_LOOP ( 'NONE', ( #23816, #1511, #13817, #25074, #6867 ) ) ;
#9750 = CARTESIAN_POINT ( 'NONE',  ( -0.03532354024591901481, -1.653543307086614345, 1.012503259137575512E-16 ) ) ;
#9751 = ORIENTED_EDGE ( 'NONE', *, *, #20623, .T. ) ;
#9752 = DIRECTION ( 'NONE',  ( 0.000000000000000000, 0.000000000000000000, 1.000000000000000000 ) ) ;
#9753 = AXIS2_PLACEMENT_3D ( 'NONE', #1287, #20777, #18207 ) ;
#9754 = SPHERICAL_SURFACE ( 'NONE', #10046, 0.1299232283464566984 ) ;
#9755 = DIRECTION ( 'NONE',  ( -0.000000000000000000, 0.000000000000000000, -1.000000000000000000 ) ) ;
#9756 = ORIENTED_EDGE ( 'NONE', *, *, #27758, .F. ) ;
#9757 = EDGE_CURVE ( 'NONE', #11845, #21446, #204, .T. ) ;
#9758 = ORIENTED_EDGE ( 'NONE', *, *, #9608, .T. ) ;
#9759 = ADVANCED_FACE ( 'NONE', ( #4292 ), #21799, .F. ) ;
#9760 = FACE_OUTER_BOUND ( 'NONE', #5863, .T. ) ;
#9761 = CARTESIAN_POINT ( 'NONE',  ( 0.1220886091262543827, -0.3369140789136257363, 0.1805249803408568721 ) ) ;
#9762 = CARTESIAN_POINT ( 'NONE',  ( -0.1771653543307086520, -5.663984251968503442E-18, 0.000000000000000000 ) ) ;
#9763 = ORIENTED_EDGE ( 'NONE', *, *, #2035, .F. ) ;
#9764 = CARTESIAN_POINT ( 'NONE',  ( -0.1570092758121678089, -0.4330450457732858416, 0.1771653543307084855 ) ) ;
#9765 = ORIENTED_EDGE ( 'NONE', *, *, #18798, .F. ) ;
#9766 = ORIENTED_EDGE ( 'NONE', *, *, #22105, .T. ) ;
#9767 = CARTESIAN_POINT ( 'NONE',  ( -0.1482986320106401412, 0.3007905576423888783, 1.973425196850393970 ) ) ;
#9768 = CARTESIAN_POINT ( 'NONE',  ( 0.4441657790094327707, -0.2564944395535760369, -1.550196850393700920 ) ) ;
#9769 = FACE_OUTER_BOUND ( 'NONE', #16732, .T. ) ;
#9770 = CARTESIAN_POINT ( 'NONE',  ( -0.4685039370078740717, 0.000000000000000000, -6.283251968503937502E-17 ) ) ;
#9771 = CARTESIAN_POINT ( 'NONE',  ( -0.03607471876262562105, -0.5511811023622046335, 0.9202755905511811330 ) ) ;
#9772 = DIRECTION ( 'NONE',  ( 0.000000000000000000, -1.000000000000000000, 0.000000000000000000 ) ) ;
#9773 = AXIS2_PLACEMENT_3D ( 'NONE', #17443, #9091, #25926 ) ;
#9774 = CARTESIAN_POINT ( 'NONE',  ( -0.3543307086367249448, 4.339299681715786259E-17, -2.322834645648385710 ) ) ;
#9775 = EDGE_LOOP ( 'NONE', ( #24301, #6819, #12896, #2814, #4943, #11835, #5030, #17505, #18697, #22390, #14010, #23296, #25147 ) ) ;
#9776 = CARTESIAN_POINT ( 'NONE',  ( -4.821444091131312140E-17, -0.3937007874015748254, 0.1771653543307086520 ) ) ;
#9777 = ADVANCED_FACE ( 'NONE', ( #6688 ), #19087, .F. ) ;
#9778 = CARTESIAN_POINT ( 'NONE',  ( -0.06441834428466612639, 0.4889536969035325753, -1.569881889763779625 ) ) ;
#9779 = CIRCLE ( 'NONE', #26443, 0.1308464566929133932 ) ;
#9780 = CARTESIAN_POINT ( 'NONE',  ( 0.3289909311256231095, -0.1896185148830507317, -3.100567304031763172 ) ) ;
#9781 = VERTEX_POINT ( 'NONE', #24050 ) ;
#9782 = MECHANICAL_DESIGN_GEOMETRIC_PRESENTATION_REPRESENTATION (  '', ( #27853 ), #1681 ) ;
#9783 = FACE_OUTER_BOUND ( 'NONE', #24580, .T. ) ;
#9784 = CARTESIAN_POINT ( 'NONE',  ( -0.06947618719668695320, 0.5280904602948609528, 1.747047244094488416 ) ) ;
#9785 = SURFACE_SIDE_STYLE ('',( #27030 ) ) ;
#9786 = CARTESIAN_POINT ( 'NONE',  ( -0.3661417322834645272, -0.4724409448818898127, -0.9954570744419902750 ) ) ;
#9787 = ORIENTED_EDGE ( 'NONE', *, *, #23893, .T. ) ;
#9788 = ORIENTED_EDGE ( 'NONE', *, *, #9346, .T. ) ;
#9789 = DIRECTION ( 'NONE',  ( -0.2036417511401762970, -0.9790454724845841783, 0.000000000000000000 ) ) ;
#9790 = CARTESIAN_POINT ( 'NONE',  ( 1.692913385826771533, 0.07874015748031491790, 3.109831496062992451E-16 ) ) ;
#9791 = EDGE_LOOP ( 'NONE', ( #16749, #23485, #24091, #27621 ) ) ;
#9792 = DIRECTION ( 'NONE',  ( 7.017815000000000124E-18, -1.000000000000000000, 0.000000000000000000 ) ) ;
#9793 = VERTEX_POINT ( 'NONE', #2435 ) ;
#9794 = CARTESIAN_POINT ( 'NONE',  ( 0.2991932138496291582, 0.3411003281196904324, -1.934055118110236338 ) ) ;
#9795 = CARTESIAN_POINT ( 'NONE',  ( 0.000000000000000000, 0.000000000000000000, -0.1377952755905511861 ) ) ;
#9796 = LINE ( 'NONE', #20539, #24199 ) ;
#9797 = CARTESIAN_POINT ( 'NONE',  ( 0.09842519685039370636, 0.2991866959364303802, -3.272637795275590733 ) ) ;
#9798 = AXIS2_PLACEMENT_3D ( 'NONE', #15973, #11867, #18344 ) ;
#9799 = CARTESIAN_POINT ( 'NONE',  ( 0.3070866141732283561, 0.000000000000000000, 0.2755905511811023723 ) ) ;
#9800 = ORIENTED_EDGE ( 'NONE', *, *, #16746, .F. ) ;
#9801 = CARTESIAN_POINT ( 'NONE',  ( -0.1968503937007874127, -0.4724409448818898127, 0.7100240035758484947 ) ) ;
#9802 = TOROIDAL_SURFACE ( 'NONE', #19266, 0.8031496062992127261, 0.02362204724409448786 ) ;
#9803 = CARTESIAN_POINT ( 'NONE',  ( 0.2118615749922464486, -0.5840192333899535404, 0.2574803149606298969 ) ) ;
#9804 = CARTESIAN_POINT ( 'NONE',  ( -0.3765118517642104257, -0.02464264302297883638, -3.100567304031763172 ) ) ;
#9805 = APPLICATION_CONTEXT ( 'automotive_design' ) ;
#9806 = VERTEX_POINT ( 'NONE', #15588 ) ;
#9807 = CARTESIAN_POINT ( 'NONE',  ( -0.2268989272875546748, 0.3929158813954828355, -1.934055118110236338 ) ) ;
#9808 = AXIS2_PLACEMENT_3D ( 'NONE', #25301, #3829, #5963 ) ;
#9809 = ADVANCED_FACE ( 'NONE', ( #24191, #19403 ), #10637, .T. ) ;
#9810 = B_SPLINE_CURVE_WITH_KNOTS ( 'NONE', 3,
 ( #11284, #4919, #13533, #15672 ),
 .UNSPECIFIED., .F., .F.,
 ( 4, 4 ),
 ( 1.726261509291350027, 1.727907812355649941 ),
 .UNSPECIFIED. ) ;
#9811 = ORIENTED_EDGE ( 'NONE', *, *, #12663, .T. ) ;
#9812 = ORIENTED_EDGE ( 'NONE', *, *, #27335, .T. ) ;
#9813 = ( GEOMETRIC_REPRESENTATION_CONTEXT ( 3 ) GLOBAL_UNCERTAINTY_ASSIGNED_CONTEXT ( ( #9585 ) ) GLOBAL_UNIT_ASSIGNED_CONTEXT ( ( #14261, #18169, #14104 ) ) REPRESENTATION_CONTEXT ( 'NONE', 'WORKASPACE' ) ) ;
#9814 = CIRCLE ( 'NONE', #8909, 0.2395669291338582696 ) ;
#9815 = CARTESIAN_POINT ( 'NONE',  ( -0.3376790527244098450, -0.7759819139694350554, -0.7889928361655353939 ) ) ;
#9816 = CARTESIAN_POINT ( 'NONE',  ( -0.6265111856126519552, -0.4592309206878726902, 0.9950886776261921307 ) ) ;
#9817 = EDGE_CURVE ( 'NONE', #27816, #22411, #2026, .T. ) ;
#9818 = CARTESIAN_POINT ( 'NONE',  ( 0.000000000000000000, 0.4941010236220472751, 0.000000000000000000 ) ) ;
#9819 = VERTEX_POINT ( 'NONE', #226 ) ;
#9820 = PRESENTATION_LAYER_ASSIGNMENT (  '', '', ( #22902 ) ) ;
#9821 = CARTESIAN_POINT ( 'NONE',  ( -0.1886891683788906593, -0.3267488823401751841, -3.100567304031762284 ) ) ;
#9822 = DIRECTION ( 'NONE',  ( 0.000000000000000000, 0.000000000000000000, 1.000000000000000000 ) ) ;
#9823 = EDGE_CURVE ( 'NONE', #3247, #7888, #7368, .T. ) ;
#9824 = CARTESIAN_POINT ( 'NONE',  ( -0.07874015748031495954, -0.04546065111729338803, -0.4724409448818898127 ) ) ;
#9825 = DIRECTION ( 'NONE',  ( -0.000000000000000000, 1.000000000000000000, -0.000000000000000000 ) ) ;
#9826 = ORIENTED_EDGE ( 'NONE', *, *, #25094, .T. ) ;
#9827 = CARTESIAN_POINT ( 'NONE',  ( -0.4251109113156978370, -0.5377216242369684540, -0.4382667117914157418 ) ) ;
#9828 = CARTESIAN_POINT ( 'NONE',  ( 0.4218945342797225662, -0.1432577568504558585, -1.934055118110236338 ) ) ;
#9829 = ORIENTED_EDGE ( 'NONE', *, *, #16589, .F. ) ;
#9830 = ORIENTED_EDGE ( 'NONE', *, *, #14866, .T. ) ;
#9831 = CARTESIAN_POINT ( 'NONE',  ( -0.7635713814939685262, 0.3957398197978322374, 0.1751423728567907401 ) ) ;
#9832 = DIRECTION ( 'NONE',  ( -0.000000000000000000, -1.000000000000000000, -0.000000000000000000 ) ) ;
#9833 = CIRCLE ( 'NONE', #24701, 0.1299212598425196763 ) ;
#9834 = FACE_BOUND ( 'NONE', #3972, .T. ) ;
#9835 = CARTESIAN_POINT ( 'NONE',  ( 0.5368353335967094297, -0.1442704874421229522, 0.9202755905511812440 ) ) ;
#9836 = AXIS2_PLACEMENT_3D ( 'NONE', #24389, #16065, #19504 ) ;
#9837 = CARTESIAN_POINT ( 'NONE',  ( 0.2676050456844303316, 0.2056553984168022209, 1.973425196850393970 ) ) ;
#9838 = CARTESIAN_POINT ( 'NONE',  ( 0.1520645003680120011, 0.1970746732787106437, 0.4530975572029189435 ) ) ;
#9839 = PRODUCT_DEFINITION_SHAPE ( 'NONE', 'NONE',  #27910 ) ;
#9840 = CARTESIAN_POINT ( 'NONE',  ( -0.09842519685039378963, 0.2165354330708661457, -3.259753967135868624 ) ) ;
#9841 = PLANE ( 'NONE',  #6701 ) ;
#9842 = AXIS2_PLACEMENT_3D ( 'NONE', #24753, #16008, #26877 ) ;
#9844 = CARTESIAN_POINT ( 'NONE',  ( 0.0006615832605804723319, 0.6212594902576319411, 0.2574803149606298969 ) ) ;
#9843 = AXIS2_PLACEMENT_3D ( 'NONE', #9183, #11734, #591 ) ;
#9845 = ORIENTED_EDGE ( 'NONE', *, *, #8377, .T. ) ;
#9846 = DIRECTION ( 'NONE',  ( -1.000000000000000000, 0.000000000000000000, 0.000000000000000000 ) ) ;
#9847 = ADVANCED_FACE ( 'NONE', ( #11061 ), #19991, .F. ) ;
#9848 = CARTESIAN_POINT ( 'NONE',  ( 0.3131893444329049703, 0.3723335979450146382, 0.2467937633107637474 ) ) ;
#9849 = FACE_OUTER_BOUND ( 'NONE', #8776, .T. ) ;
#9850 = CARTESIAN_POINT ( 'NONE',  ( 0.03478633594543729946, 0.5314960629921260393, 1.747047244094488194 ) ) ;
#9851 = EDGE_CURVE ( 'NONE', #12340, #27804, #23789, .T. ) ;
#9852 = VECTOR ( 'NONE', #12379, 39.37007874015748143 ) ;
#9853 = ORIENTED_EDGE ( 'NONE', *, *, #16536, .T. ) ;
#9854 = AXIS2_PLACEMENT_3D ( 'NONE', #20591, #18448, #8030 ) ;
#9855 = CARTESIAN_POINT ( 'NONE',  ( -0.3334645669291338987, 0.8151331854455394765, -1.007197927683596506 ) ) ;
#9856 = ORIENTED_EDGE ( 'NONE', *, *, #1800, .T. ) ;
#9857 = EDGE_CURVE ( 'NONE', #14224, #11946, #4432, .T. ) ;
#9858 = DIRECTION ( 'NONE',  ( 1.000000000000000000, 7.017815000000000124E-18, 0.000000000000000000 ) ) ;
#9859 = ( NAMED_UNIT ( * ) SI_UNIT ( $, .STERADIAN. ) SOLID_ANGLE_UNIT ( ) ) ;
#9860 = DIRECTION ( 'NONE',  ( 0.000000000000000000, 0.000000000000000000, 1.000000000000000000 ) ) ;
#9861 = DIRECTION ( 'NONE',  ( -1.000000000000000000, 0.000000000000000000, 0.000000000000000000 ) ) ;
#9862 = EDGE_LOOP ( 'NONE', ( #7543, #20401, #18259, #17249 ) ) ;
#9863 = EDGE_LOOP ( 'NONE', ( #27140, #14100, #2285, #15497, #2424, #11097, #18670, #6412, #3178, #8412, #22798 ) ) ;
#9864 = CARTESIAN_POINT ( 'NONE',  ( 0.4889536969035315206, 0.06441834428467128892, -1.569881889763779625 ) ) ;
#9865 = AXIS2_PLACEMENT_3D ( 'NONE', #19355, #54, #8620 ) ;
#9866 = ORIENTED_EDGE ( 'NONE', *, *, #15668, .F. ) ;
#9867 = EDGE_LOOP ( 'NONE', ( #19076, #4872, #18206, #8995 ) ) ;
#9868 = EDGE_CURVE ( 'NONE', #21006, #10381, #1647, .T. ) ;
#9869 = CONTEXT_DEPENDENT_SHAPE_REPRESENTATION ( #3101, #24028 ) ;
#9870 = EDGE_LOOP ( 'NONE', ( #14412, #13682, #19670, #20142 ) ) ;
#9871 = DIRECTION ( 'NONE',  ( 0.000000000000000000, -1.000000000000000000, 0.000000000000000000 ) ) ;
#9872 = CARTESIAN_POINT ( 'NONE',  ( -0.3149606299212598381, 0.000000000000000000, 0.000000000000000000 ) ) ;
#9873 = CARTESIAN_POINT ( 'NONE',  ( 0.4621951630817700551, 0.08130208312399862802, 0.1992150590373740204 ) ) ;
#9874 = AXIS2_PLACEMENT_3D ( 'NONE', #15077, #4966, #24318 ) ;
#9875 = CIRCLE ( 'NONE', #1772, 0.6881889763779527325 ) ;
#9876 = ORIENTED_EDGE ( 'NONE', *, *, #18551, .T. ) ;
#9877 = DIRECTION ( 'NONE',  ( 0.000000000000000000, 0.000000000000000000, 1.000000000000000000 ) ) ;
#9878 = AXIS2_PLACEMENT_3D ( 'NONE', #10121, #8020, #21004 ) ;
#9879 = UNCERTAINTY_MEASURE_WITH_UNIT (LENGTH_MEASURE( 1.000000000000000082E-05 ), #9609, 'distance_accuracy_value', 'NONE') ;
#9880 = VERTEX_POINT ( 'NONE', #26856 ) ;
#9881 = LINE ( 'NONE', #24567, #2395 ) ;
#9882 = CARTESIAN_POINT ( 'NONE',  ( 0.4061284506584276199, -0.2351468520616558922, 0.07637795275590551769 ) ) ;
#9883 = CARTESIAN_POINT ( 'NONE',  ( -0.1771653543307086520, -5.663984251968503442E-18, 0.000000000000000000 ) ) ;
#9884 = AXIS2_PLACEMENT_3D ( 'NONE', #14045, #20538, #24617 ) ;
#9885 = CARTESIAN_POINT ( 'NONE',  ( 0.2122766679520079192, -0.5838685267775929333, 0.2574827755769819038 ) ) ;
#9886 = DIRECTION ( 'NONE',  ( 0.000000000000000000, 0.000000000000000000, 1.000000000000000000 ) ) ;
#9887 = ADVANCED_FACE ( 'NONE', ( #18068 ), #8270, .F. ) ;
#9888 = CIRCLE ( 'NONE', #16389, 0.7874015748031496509 ) ;
#9889 = ORIENTED_EDGE ( 'NONE', *, *, #19531, .F. ) ;
#9890 = EDGE_LOOP ( 'NONE', ( #4341, #4015 ) ) ;
#9891 = CIRCLE ( 'NONE', #10806, 1.131889763779527547 ) ;
#9892 = EDGE_LOOP ( 'NONE', ( #11009, #2047, #13091, #7761 ) ) ;
#9893 = VECTOR ( 'NONE', #15625, 39.37007874015748143 ) ;
#9894 = DIRECTION ( 'NONE',  ( 0.000000000000000000, 0.000000000000000000, 1.000000000000000000 ) ) ;
#9895 = CARTESIAN_POINT ( 'NONE',  ( 0.4035433070866141780, 0.000000000000000000, 0.000000000000000000 ) ) ;
#9896 = AXIS2_PLACEMENT_3D ( 'NONE', #23491, #25593, #13140 ) ;
#9897 = CARTESIAN_POINT ( 'NONE',  ( 0.01030706208231913640, 0.1968503937007873850, -3.626968503937007871 ) ) ;
#9898 = EDGE_LOOP ( 'NONE', ( #20575, #24690, #8835, #23811, #19853, #22471, #6532, #25734, #17240, #9327, #19481, #5089, #1339, #22898, #5124, #19598, #25151, #23883, #20480 ) ) ;
#9899 = CYLINDRICAL_SURFACE ( 'NONE', #13742, 0.3937007874015748254 ) ;
#9900 = CARTESIAN_POINT ( 'NONE',  ( 0.000000000000000000, 0.1968503937007875237, -1.377952755905512472 ) ) ;
#9901 = ORIENTED_EDGE ( 'NONE', *, *, #24366, .F. ) ;
#9902 = SURFACE_STYLE_USAGE ( .BOTH. , #16403 ) ;
#9903 = DIRECTION ( 'NONE',  ( -7.017815000000000124E-18, 1.000000000000000000, -1.224646799147353207E-16 ) ) ;
#9904 = CARTESIAN_POINT ( 'NONE',  ( -0.6299212598425196763, 0.000000000000000000, 0.000000000000000000 ) ) ;
#9905 = CARTESIAN_POINT ( 'NONE',  ( 0.000000000000000000, 0.000000000000000000, 0.4488188976377953110 ) ) ;
#9906 = CARTESIAN_POINT ( 'NONE',  ( -0.6514872030428984218, 0.1141809932450963266, 0.1926811207670676152 ) ) ;
#9907 = ORIENTED_EDGE ( 'NONE', *, *, #2729, .F. ) ;
#9908 = DIRECTION ( 'NONE',  ( 1.000000000000000000, 0.000000000000000000, 0.000000000000000000 ) ) ;
#9909 = CARTESIAN_POINT ( 'NONE',  ( -0.2564944395535628252, -0.4441657790094413749, -1.550196850393700920 ) ) ;
#9910 = AXIS2_PLACEMENT_3D ( 'NONE', #915, #5278, #15876 ) ;
#9911 = CARTESIAN_POINT ( 'NONE',  ( 0.5511811023622047445, 0.07214943758244277139, 0.9202755905511812440 ) ) ;
#9912 = ADVANCED_FACE ( 'NONE', ( #16136 ), #7825, .T. ) ;
#9913 = CIRCLE ( 'NONE', #13494, 0.01968503937007875723 ) ;
#9914 = CARTESIAN_POINT ( 'NONE',  ( -0.3642352168757361786, -0.4152525734086467968, 0.9202755905511811330 ) ) ;
#9915 = DIRECTION ( 'NONE',  ( -1.000000000000000000, 0.000000000000000000, 0.000000000000000000 ) ) ;
#9916 = ORIENTED_EDGE ( 'NONE', *, *, #17896, .T. ) ;
#9917 = CARTESIAN_POINT ( 'NONE',  ( -0.2311492806687369950, -0.4794744477484330636, 0.3401599409343964431 ) ) ;
#9918 = EDGE_CURVE ( 'NONE', #20576, #6454, #15496, .T. ) ;
#9919 = CARTESIAN_POINT ( 'NONE',  ( 0.04928528614549709808, -0.3765118517642105367, -3.100567304031763616 ) ) ;
#9920 = CARTESIAN_POINT ( 'NONE',  ( 0.000000000000000000, 0.5322834645669292097, 0.3401599409343964431 ) ) ;
#9921 = ORIENTED_EDGE ( 'NONE', *, *, #13543, .F. ) ;
#9922 = DIRECTION ( 'NONE',  ( 0.000000000000000000, 0.000000000000000000, 1.000000000000000000 ) ) ;
#9923 = CARTESIAN_POINT ( 'NONE',  ( -0.1771653543307086520, -5.663984251968503442E-18, 0.000000000000000000 ) ) ;
#9924 = DIRECTION ( 'NONE',  ( -0.7818314824680302477, -0.6234898018587331503, 0.000000000000000000 ) ) ;
#9925 = DIRECTION ( 'NONE',  ( -0.2036417511401762970, 0.9790454724845841783, -1.198984999999999849E-16 ) ) ;
#9926 = ORIENTED_EDGE ( 'NONE', *, *, #10677, .F. ) ;
#9927 = VECTOR ( 'NONE', #8521, 39.37007874015748854 ) ;
#9928 = CARTESIAN_POINT ( 'NONE',  ( -0.0007595033562148819414, 0.6881885572739390167, 0.1322834645669291320 ) ) ;
#9929 = VERTEX_POINT ( 'NONE', #20082 ) ;
#9930 = CARTESIAN_POINT ( 'NONE',  ( -0.4216927985375814592, -0.2427835582314765150, 0.09284957166320603750 ) ) ;
#9931 = CIRCLE ( 'NONE', #4522, 0.3332647802741406373 ) ;
#9932 = FACE_OUTER_BOUND ( 'NONE', #24940, .T. ) ;
#9933 = DIRECTION ( 'NONE',  ( 0.000000000000000000, 0.8660254037844385966, 0.4999999999999998335 ) ) ;
#9934 = CARTESIAN_POINT ( 'NONE',  ( 0.3715251363271980245, 0.06498290224717499786, 0.07637795275590551769 ) ) ;
#9935 = DIRECTION ( 'NONE',  ( 0.000000000000000000, 0.000000000000000000, 1.000000000000000000 ) ) ;
#9936 = DIRECTION ( 'NONE',  ( 0.000000000000000000, -0.8660254037844385966, -0.4999999999999998335 ) ) ;
#9937 = ORIENTED_EDGE ( 'NONE', *, *, #13522, .T. ) ;
#9938 = CARTESIAN_POINT ( 'NONE',  ( -0.1870078740157480324, -0.8267716535433071723, 1.012503259137575512E-16 ) ) ;
#9939 = LINE ( 'NONE', #5719, #21912 ) ;
#9940 = COLOUR_RGB ( '', 0.09019608, 0.27058824, 0.51372549) ;
#9941 = CARTESIAN_POINT ( 'NONE',  ( -0.5905511811023621549, 0.9448818897637796255, -0.1771653543307086520 ) ) ;
#9942 = B_SPLINE_CURVE_WITH_KNOTS ( 'NONE', 3,
 ( #11618, #3131, #20241, #22643, #26448, #13884 ),
 .UNSPECIFIED., .F., .F.,
 ( 4, 2, 4 ),
 ( 0.9031406754215579591, 0.9046454396443720514, 0.9061502038671860326 ),
 .UNSPECIFIED. ) ;
#9943 = CARTESIAN_POINT ( 'NONE',  ( 0.1151354519024844064, -0.3392634445560540057, -3.115157480314960203 ) ) ;
#9944 = PRODUCT_DEFINITION_CONTEXT ( 'detailed design', #21908, 'design' ) ;
#9945 = ORIENTED_EDGE ( 'NONE', *, *, #3524, .T. ) ;
#9946 = CARTESIAN_POINT ( 'NONE',  ( 0.2228126397719810137, -0.3858397471888643793, -1.934055118110236338 ) ) ;
#9947 = EDGE_CURVE ( 'NONE', #8687, #24154, #20224, .T. ) ;
#9948 = LENGTH_MEASURE_WITH_UNIT ( LENGTH_MEASURE( 0.02539999999999999897 ), #16321 ) ;
#9949 = TOROIDAL_SURFACE ( 'NONE', #2273, 0.5610236220472440971, 0.1003937007874015908 ) ;
#9950 = ORIENTED_EDGE ( 'NONE', *, *, #21075, .F. ) ;
#9951 = ORIENTED_EDGE ( 'NONE', *, *, #13257, .T. ) ;
#9952 = CARTESIAN_POINT ( 'NONE',  ( -0.4473595089310440920, -0.6685828274113149172, -0.1391927031366795575 ) ) ;
#9953 = FACE_OUTER_BOUND ( 'NONE', #8397, .T. ) ;
#9954 = EDGE_LOOP ( 'NONE', ( #20171, #20807, #2244, #7861 ) ) ;
#9955 = DIRECTION ( 'NONE',  ( 0.000000000000000000, 0.000000000000000000, 1.000000000000000000 ) ) ;
#9956 = VERTEX_POINT ( 'NONE', #5536 ) ;
#9957 = CIRCLE ( 'NONE', #14507, 0.7539370078740157410 ) ;
#9958 = CARTESIAN_POINT ( 'NONE',  ( 0.000000000000000000, 0.000000000000000000, -4.330708661417323135 ) ) ;
#9959 = FACE_OUTER_BOUND ( 'NONE', #23656, .T. ) ;
#9960 = DIRECTION ( 'NONE',  ( 0.000000000000000000, 0.000000000000000000, 1.000000000000000000 ) ) ;
#9961 = ORIENTED_EDGE ( 'NONE', *, *, #13512, .T. ) ;
#9962 = CARTESIAN_POINT ( 'NONE',  ( 0.1285103288269283661, -0.3545966721392122545, 0.1992125984251968684 ) ) ;
#9963 = CARTESIAN_POINT ( 'NONE',  ( -1.197070535079588716, 0.07874015748031491790, 1.197070535079588716 ) ) ;
#9964 = ( REPRESENTATION_RELATIONSHIP ('NONE','NONE', #12434, #22737 ) REPRESENTATION_RELATIONSHIP_WITH_TRANSFORMATION ( #8183 )SHAPE_REPRESENTATION_RELATIONSHIP( ) ) ;
#9965 = ORIENTED_EDGE ( 'NONE', *, *, #10875, .T. ) ;
#9966 = ORIENTED_EDGE ( 'NONE', *, *, #5617, .T. ) ;
#9967 = ORIENTED_EDGE ( 'NONE', *, *, #25976, .T. ) ;
#9968 = VERTEX_POINT ( 'NONE', #22064 ) ;
#9969 = APPLICATION_CONTEXT ( 'automotive_design' ) ;
#9970 = CARTESIAN_POINT ( 'NONE',  ( -0.1968503937007874127, 1.355271913027328057E-17, 0.1476377952755905387 ) ) ;
#9971 = FACE_BOUND ( 'NONE', #9285, .T. ) ;
#9972 = B_SPLINE_CURVE_WITH_KNOTS ( 'NONE', 3,
 ( #22348, #26717, #13873, #1437, #22492, #11894, #3393, #3121 ),
 .UNSPECIFIED., .F., .F.,
 ( 4, 2, 2, 4 ),
 ( 0.000000000000000000, 0.1250000000000001110, 0.2500000000000002220, 0.5000000000000000000 ),
 .UNSPECIFIED. ) ;
#9973 = EDGE_CURVE ( 'NONE', #21357, #23265, #23632, .T. ) ;
#9974 = CARTESIAN_POINT ( 'NONE',  ( 0.3551931031211721379, 0.04679574315772513232, -3.115157480314960647 ) ) ;
#9975 = DIRECTION ( 'NONE',  ( 1.000000000000000000, 0.000000000000000000, 0.000000000000000000 ) ) ;
#9976 = CARTESIAN_POINT ( 'NONE',  ( 0.04380501567505448723, 0.3346456692913385988, 1.973425196850394192 ) ) ;
#9977 = CARTESIAN_POINT ( 'NONE',  ( -0.2490711204941342405, 1.208528701367826752, -0.6047752023237676910 ) ) ;
#9978 = AXIS2_PLACEMENT_3D ( 'NONE', #2795, #2937, #17781 ) ;
#9979 = FACE_OUTER_BOUND ( 'NONE', #16010, .T. ) ;
#9980 = CIRCLE ( 'NONE', #5948, 0.8267716535433071723 ) ;
#9981 = DIRECTION ( 'NONE',  ( 0.000000000000000000, 0.000000000000000000, -1.000000000000000000 ) ) ;
#9983 = ADVANCED_FACE ( 'NONE', ( #1164 ), #9614, .F. ) ;
#9982 = AXIS2_PLACEMENT_3D ( 'NONE', #10313, #18935, #12448 ) ;
#9984 = CARTESIAN_POINT ( 'NONE',  ( -0.3020979083623086536, 0.3591256245825952265, 0.07637795275590551769 ) ) ;
#9985 = DIRECTION ( 'NONE',  ( 1.000000000000000000, 0.000000000000000000, 0.000000000000000000 ) ) ;
#9986 = ORIENTED_EDGE ( 'NONE', *, *, #8296, .T. ) ;
#9987 = CARTESIAN_POINT ( 'NONE',  ( -0.4301590433675065994, 0.3771696032820260336, 0.9399606299212601712 ) ) ;
#9988 = CARTESIAN_POINT ( 'NONE',  ( -0.5949363243629232079, -0.1357903337134990229, 0.3661437007874016047 ) ) ;
#9989 = ORIENTED_EDGE ( 'NONE', *, *, #27181, .F. ) ;
#9990 = DIRECTION ( 'NONE',  ( 0.000000000000000000, 0.000000000000000000, 1.000000000000000000 ) ) ;
#9991 = FACE_OUTER_BOUND ( 'NONE', #3199, .T. ) ;
#9992 = CARTESIAN_POINT ( 'NONE',  ( 0.3512268162760394108, 0.4004221243553300891, 1.747047244094488194 ) ) ;
#9993 = CARTESIAN_POINT ( 'NONE',  ( -0.09842519685039370636, 0.2165354330708661457, -3.272637795275590733 ) ) ;
#9994 = CARTESIAN_POINT ( 'NONE',  ( -0.4069448477556107946, -0.3121994997598286914, 1.766732283464566899 ) ) ;
#9995 = ORIENTED_EDGE ( 'NONE', *, *, #5881, .T. ) ;
#9996 = AXIS2_PLACEMENT_3D ( 'NONE', #10633, #19256, #4014 ) ;
#9997 = VERTEX_POINT ( 'NONE', #26708 ) ;
#9998 = CARTESIAN_POINT ( 'NONE',  ( 0.1318897637674579792, 0.000000000000000000, 0.9055118110027171596 ) ) ;
#9999 = ORIENTED_EDGE ( 'NONE', *, *, #24672, .T. ) ;
#10000 = CARTESIAN_POINT ( 'NONE',  ( 0.000000000000000000, 0.000000000000000000, -0.05511811023622047168 ) ) ;
#10001 = CARTESIAN_POINT ( 'NONE',  ( -0.4303822302054170490, 0.1152775731717081975, -1.934055118110236338 ) ) ;
#10002 = CARTESIAN_POINT ( 'NONE',  ( 0.3769281224616271575, 0.7313191576793038884, -0.6886840467356212248 ) ) ;
#10003 = FACE_OUTER_BOUND ( 'NONE', #5027, .T. ) ;
#10004 = VERTEX_POINT ( 'NONE', #11744 ) ;
#10005 = AXIS2_PLACEMENT_3D ( 'NONE', #18643, #5961, #8215 ) ;
#10006 = EDGE_LOOP ( 'NONE', ( #7620, #7939 ) ) ;
#10007 = CONICAL_SURFACE ( 'NONE', #16791, 65.52281417845038902, 1.029744258088330700 ) ;
#10008 = CARTESIAN_POINT ( 'NONE',  ( -0.4270824798167697223, -0.2466292688015108703, -1.569881889763779625 ) ) ;
#10009 = ORIENTED_EDGE ( 'NONE', *, *, #19680, .T. ) ;
#10010 = EDGE_CURVE ( 'NONE', #23052, #27804, #26739, .T. ) ;
#10011 = B_SPLINE_CURVE_WITH_KNOTS ( 'NONE', 3,
 ( #4853, #8689, #2725, #15355, #11358, #15203 ),
 .UNSPECIFIED., .F., .F.,
 ( 4, 2, 4 ),
 ( 0.2291966065698859967, 0.2305109203526899964, 0.2318252341354939960 ),
 .UNSPECIFIED. ) ;
#10012 = CARTESIAN_POINT ( 'NONE',  ( -0.3432721300517010965, 0.06002180498082090171, 0.1589462317926021162 ) ) ;
#10013 = EDGE_CURVE ( 'NONE', #5387, #27620, #3763, .T. ) ;
#10014 = CARTESIAN_POINT ( 'NONE',  ( 0.4620947063919622066, 0.08187111969652538512, 0.1992142434433712694 ) ) ;
#10015 = CARTESIAN_POINT ( 'NONE',  ( -0.4620608682196346573, 0.08206165078060512208, 0.1992125984251968684 ) ) ;
#10016 = B_SPLINE_SURFACE_WITH_KNOTS ( 'NONE', 2, 3, ( 
 ( #13270, #4780, #21894, #7464, #16092, #15942, #22440, #7186, #13976, #2929, #14111, #22722, #27113, #18609, #11992, #3493, #24686, #15805, #18463, #24411, #3350, #20322, #7759, #20607, #5199, #9426, #5057, #18027, #20174, #5500, #13826, #9864, #24976, #1260, #16371, #20465, #5349, #18174, #3064, #22875, #24835, #18323, #24545, #11699, #13678, #979, #9723, #26668, #9565, #26815, #22295, #22585, #3210, #11843, #5637, #1123, #26968, #12125, #11558, #10008, #7616, #7323, #16235, #14267, #836, #20749 ),
 ( #1390, #12411, #21024, #10705, #21169, #14409, #10278, #23017, #2093, #1812, #6341, #3935, #8177, #4217, #19039, #27251, #4077, #12552, #21455, #12823, #6209, #21312, #14702, #17071, #10420, #20885, #23448, #19183, #25688, #3637, #23308, #27391, #16502, #8320, #12265, #14970, #16939, #7898, #23585, #6067, #27814, #3791, #16792, #25549, #8447, #1532, #25120, #10139, #5785, #1671, #8044, #18892, #16652, #5925, #14560, #23157, #25404, #5985, #2282, #18811, #19246, #27738, #4277, #27594, #25322, #23778 ),
 ( #18958, #12470, #8237, #3999, #6402, #23220, #15029, #8099, #12881, #21373, #19386, #21233, #1872, #16709, #12743, #14619, #10480, #3852, #21652, #2009, #25889, #23507, #8380, #4420, #10620, #21083, #21515, #4136, #13024, #1731, #25750, #2152, #6261, #8647, #27876, #10343, #82, #6535, #15167, #16859, #14898, #25469, #6131, #8510, #19100, #16995, #17130, #25607, #6814, #11314, #24036, #4674, #25003, #22903, #27272, #11874, #27703, #23189, #23045, #25435, #6233, #6101, #3820, #1700, #10307, #8207 ) ),
 .UNSPECIFIED., .F., .T., .F.,
 ( 3, 3 ),
 ( 4, 2, 2, 2, 2, 2, 2, 2, 2, 2, 2, 2, 2, 2, 2, 2, 2, 2, 2, 2, 2, 2, 2, 2, 2, 2, 2, 2, 2, 2, 2, 2, 4 ),
 ( 0.000000000000000000, 1.000000000000000000 ),
 ( 0.000000000000000000, 0.1963495408493620697, 0.3926990816987241395, 0.5890486225480862092, 0.7853981633974482790, 0.9817477042468103487, 1.178097245096172418, 1.374446785945534488, 1.570796326794896558, 1.767145867644258628, 1.963495408493620697, 2.159844949342982545, 2.356194490192344837, 2.552544031041707129, 2.748893571891068976, 2.945243112740430824, 3.141592653589793116, 3.337942194439155408, 3.534291735288517255, 3.730641276137879103, 3.926990816987241395, 4.123340357836603687, 4.319689898685965090, 4.516039439535327382, 4.712388980384689674, 4.908738521234051966, 5.105088062083414258, 5.301437602932775661, 5.497787143782137953, 5.694136684631500245, 5.890486225480861648, 6.086835766330223940, 6.283185307179586232 ),
 .UNSPECIFIED. ) ;
#10017 = EDGE_CURVE ( 'NONE', #14224, #13094, #11419, .T. ) ;
#10018 = CIRCLE ( 'NONE', #8669, 0.4941010236220472751 ) ;
#10019 = ORIENTED_EDGE ( 'NONE', *, *, #22804, .T. ) ;
#10020 = CARTESIAN_POINT ( 'NONE',  ( -0.5905511811023621549, 0.9448818897637796255, 0.1771653543307086520 ) ) ;
#10021 = ADVANCED_FACE ( 'NONE', ( #7225 ), #1508, .F. ) ;
#10022 = DIRECTION ( 'NONE',  ( -1.000000000000000000, 0.000000000000000000, 0.000000000000000000 ) ) ;
#10023 = CARTESIAN_POINT ( 'NONE',  ( -0.5905511811023621549, 0.9104330708661417804, 0.000000000000000000 ) ) ;
#10024 = CARTESIAN_POINT ( 'NONE',  ( -0.6081663209497759626, -0.1717464423132456786, 0.2247343301158596096 ) ) ;
#10025 = CARTESIAN_POINT ( 'NONE',  ( 0.2118615749922464486, -0.5840192333899535404, 0.2574803149606298969 ) ) ;
#10026 = FACE_OUTER_BOUND ( 'NONE', #2017, .T. ) ;
#10027 = ORIENTED_EDGE ( 'NONE', *, *, #17078, .T. ) ;
#10028 = ORIENTED_EDGE ( 'NONE', *, *, #3343, .F. ) ;
#10029 = AXIS2_PLACEMENT_3D ( 'NONE', #22224, #19969, #17577 ) ;
#10030 = VERTEX_POINT ( 'NONE', #2830 ) ;
#10031 = CARTESIAN_POINT ( 'NONE',  ( 0.000000000000000000, -0.4941010236220472751, 6.050992370341708321E-17 ) ) ;
#10032 = DIRECTION ( 'NONE',  ( 1.000000000000000000, 0.000000000000000000, 0.000000000000000000 ) ) ;
#10033 = CARTESIAN_POINT ( 'NONE',  ( 0.000000000000000000, 0.3543307086614173040, 0.000000000000000000 ) ) ;
#10034 = VERTEX_POINT ( 'NONE', #7654 ) ;
#10035 = DIRECTION ( 'NONE',  ( 1.000000000000000000, 0.000000000000000000, 0.000000000000000000 ) ) ;
#10036 = EDGE_LOOP ( 'NONE', ( #11650, #17799, #17741, #12878 ) ) ;
#10037 = ADVANCED_FACE ( 'NONE', ( #17814 ), #1958, .F. ) ;
#10038 = CIRCLE ( 'NONE', #17712, 0.5893189861902062843 ) ;
#10039 = CARTESIAN_POINT ( 'NONE',  ( 0.7874015748031496509, -5.862181872755905604E-06, -1.869015748010449007 ) ) ;
#10040 = CARTESIAN_POINT ( 'NONE',  ( -0.0005847768872418040737, 0.4787829797941598464, 0.1920935997050576827 ) ) ;
#10041 = CARTESIAN_POINT ( 'NONE',  ( -8.632637795275590524E-16, -0.07677165354330710290, 0.000000000000000000 ) ) ;
#10042 = ADVANCED_FACE ( 'NONE', ( #16273 ), #27224, .T. ) ;
#10043 = CARTESIAN_POINT ( 'NONE',  ( 3.644242538420618632E-18, 0.5007874015748032814, 0.09684793308443545579 ) ) ;
#10044 = CARTESIAN_POINT ( 'NONE',  ( 0.000000000000000000, 0.000000000000000000, -3.149606299191693548 ) ) ;
#10045 = CARTESIAN_POINT ( 'NONE',  ( 0.2211428102655695338, -0.2521176338356630464, 1.973425196850393970 ) ) ;
#10046 = AXIS2_PLACEMENT_3D ( 'NONE', #15978, #8045, #21313 ) ;
#10047 = DIRECTION ( 'NONE',  ( 0.000000000000000000, 1.000000000000000000, 0.000000000000000000 ) ) ;
#10048 = VECTOR ( 'NONE', #18546, 39.37007874015748854 ) ;
#10049 = CARTESIAN_POINT ( 'NONE',  ( -0.4152525734085961151, -0.3642352168756899933, 0.9399606299212598381 ) ) ;
#10050 = DIRECTION ( 'NONE',  ( 1.000000000000000000, 0.000000000000000000, 0.000000000000000000 ) ) ;
#10051 = CARTESIAN_POINT ( 'NONE',  ( 0.6299212598425196763, 0.000000000000000000, 0.000000000000000000 ) ) ;
#10052 = ORIENTED_EDGE ( 'NONE', *, *, #13853, .T. ) ;
#10053 = CARTESIAN_POINT ( 'NONE',  ( -0.02916473398703043826, 0.07408303521633090305, -0.4653527282821431355 ) ) ;
#10054 = TOROIDAL_SURFACE ( 'NONE', #24485, 0.3584231247409862542, 0.01377952755905511792 ) ;
#10055 = CARTESIAN_POINT ( 'NONE',  ( 0.03937007874015747977, 0.000000000000000000, 0.000000000000000000 ) ) ;
#10056 = CARTESIAN_POINT ( 'NONE',  ( 0.07669076177804119709, 0.1968503937007873850, -3.252027725244190481 ) ) ;
#10057 = CARTESIAN_POINT ( 'NONE',  ( 0.5314960629921261503, 0.03490580340508878110, 1.747047244094489304 ) ) ;
#10058 = VERTEX_POINT ( 'NONE', #15715 ) ;
#10059 = CARTESIAN_POINT ( 'NONE',  ( -0.7086614173228346081, 0.000000000000000000, -1.200787401574803237 ) ) ;
#10060 = DIRECTION ( 'NONE',  ( 0.000000000000000000, 0.000000000000000000, -1.000000000000000000 ) ) ;
#10061 = DIRECTION ( 'NONE',  ( 0.000000000000000000, 0.000000000000000000, 1.000000000000000000 ) ) ;
#10062 = DIRECTION ( 'NONE',  ( 0.000000000000000000, 0.000000000000000000, -1.000000000000000000 ) ) ;
#10063 = ORIENTED_EDGE ( 'NONE', *, *, #1754, .T. ) ;
#10064 = TOROIDAL_SURFACE ( 'NONE', #6918, 0.6102362204724409711, 0.1299212598425196763 ) ;
#10065 = CARTESIAN_POINT ( 'NONE',  ( -1.466875984251968630E-17, 0.000000000000000000, 0.000000000000000000 ) ) ;
#10066 = ORIENTED_EDGE ( 'NONE', *, *, #17947, .T. ) ;
#10067 = EDGE_CURVE ( 'NONE', #16467, #27805, #22202, .T. ) ;
#10068 = AXIS2_PLACEMENT_3D ( 'NONE', #885, #22487, #7509 ) ;
#10069 = DIRECTION ( 'NONE',  ( 0.000000000000000000, 0.000000000000000000, -1.000000000000000000 ) ) ;
#10070 = FACE_OUTER_BOUND ( 'NONE', #2427, .T. ) ;
#10071 = EDGE_CURVE ( 'NONE', #11604, #25393, #9154, .T. ) ;
#10072 = CARTESIAN_POINT ( 'NONE',  ( 0.07874015748031489015, 9.642888182262615344E-18, -0.2834645669291338543 ) ) ;
#10073 = CARTESIAN_POINT ( 'NONE',  ( 0.000000000000000000, 0.000000000000000000, -0.3740157480314960647 ) ) ;
#10074 = CARTESIAN_POINT ( 'NONE',  ( 0.1279527559055118058, 0.000000000000000000, 0.000000000000000000 ) ) ;
#10075 = EDGE_CURVE ( 'NONE', #2155, #18698, #16695, .T. ) ;
#10076 = ORIENTED_EDGE ( 'NONE', *, *, #1693, .T. ) ;
#10077 = CARTESIAN_POINT ( 'NONE',  ( -0.2126900928101220500, -0.5837180524351338606, 0.2574827755769819038 ) ) ;
#10078 = DIRECTION ( 'NONE',  ( -1.000000000000000000, 0.000000000000000000, 0.000000000000000000 ) ) ;
#10079 = VECTOR ( 'NONE', #2238, 39.37007874015748143 ) ;
#10080 = DIRECTION ( 'NONE',  ( 0.000000000000000000, -1.000000000000000000, 0.000000000000000000 ) ) ;
#10081 = CIRCLE ( 'NONE', #26770, 0.6299212598425196763 ) ;
#10082 = ORIENTED_EDGE ( 'NONE', *, *, #21507, .F. ) ;
#10083 = CARTESIAN_POINT ( 'NONE',  ( 0.3392608232658640977, -0.1151343661288334597, -3.115157480314961091 ) ) ;
#10084 = ORIENTED_EDGE ( 'NONE', *, *, #19042, .T. ) ;
#10085 = CARTESIAN_POINT ( 'NONE',  ( -0.1432577568504724008, -0.4218945342797531528, -1.934055118110236338 ) ) ;
#10086 = CARTESIAN_POINT ( 'NONE',  ( -0.4527559054764770385, -0.02963280468031422032, -1.934055118110236338 ) ) ;
#10087 = EDGE_CURVE ( 'NONE', #27463, #6066, #26908, .T. ) ;
#10088 = EDGE_LOOP ( 'NONE', ( #8504, #14497, #26757, #12288 ) ) ;
#10089 = ORIENTED_EDGE ( 'NONE', *, *, #6118, .T. ) ;
#10090 = ORIENTED_EDGE ( 'NONE', *, *, #16372, .T. ) ;
#10091 = CARTESIAN_POINT ( 'NONE',  ( 0.5501272682997877528, 0.4396946356868946526, 0.3281099440176548088 ) ) ;
#10092 = DIRECTION ( 'NONE',  ( 0.000000000000000000, 0.000000000000000000, -1.000000000000000000 ) ) ;
#10093 = CARTESIAN_POINT ( 'NONE',  ( 0.5314960629921260393, 0.000000000000000000, 1.747047244094488194 ) ) ;
#10094 = ORIENTED_EDGE ( 'NONE', *, *, #25062, .F. ) ;
#10095 = DIRECTION ( 'NONE',  ( 0.000000000000000000, 0.000000000000000000, 1.000000000000000000 ) ) ;
#10096 = ORIENTED_EDGE ( 'NONE', *, *, #12786, .T. ) ;
#10097 = CIRCLE ( 'NONE', #21403, 0.01377952755905510404 ) ;
#10098 = CARTESIAN_POINT ( 'NONE',  ( 0.3765118517642104257, -0.02464264302293790732, -3.100567304031763172 ) ) ;
#10099 = CIRCLE ( 'NONE', #17327, 0.1771653543307086520 ) ;
#10100 = CARTESIAN_POINT ( 'NONE',  ( 0.000000000000000000, 0.000000000000000000, -1.550196850393700920 ) ) ;
#10101 = CARTESIAN_POINT ( 'NONE',  ( -0.5385210225480960844, 0.4284847435812472183, 0.1322834645669291320 ) ) ;
#10102 = CARTESIAN_POINT ( 'NONE',  ( -0.2161381151962937508, 0.2817310484609270027, 1.953740157480315043 ) ) ;
#10103 = ORIENTED_EDGE ( 'NONE', *, *, #11571, .F. ) ;
#10104 = CARTESIAN_POINT ( 'NONE',  ( -1.197070535079588716, 0.07874015748031495954, 1.078960298859116707 ) ) ;
#10106 = CARTESIAN_POINT ( 'NONE',  ( 0.2762247810518927427, -0.4783323773986943306, 0.9399606299212598381 ) ) ;
#10105 = DIRECTION ( 'NONE',  ( -0.7660444431189775694, 0.6427876096865401401, 0.000000000000000000 ) ) ;
#10107 = FACE_OUTER_BOUND ( 'NONE', #17685, .T. ) ;
#10108 = ORIENTED_EDGE ( 'NONE', *, *, #4159, .F. ) ;
#10109 = ORIENTED_EDGE ( 'NONE', *, *, #23236, .T. ) ;
#10110 = DIRECTION ( 'NONE',  ( 0.000000000000000000, 0.000000000000000000, 1.000000000000000000 ) ) ;
#10111 = CARTESIAN_POINT ( 'NONE',  ( -0.4055118110236220486, -0.4724409448818898127, -0.9954570744419902750 ) ) ;
#10112 = ADVANCED_FACE ( 'NONE', ( #22760, #3385 ), #12593, .T. ) ;
#10113 = VECTOR ( 'NONE', #4270, 39.37007874015748143 ) ;
#10114 = EDGE_CURVE ( 'NONE', #19539, #24735, #600, .T. ) ;
#10115 = CARTESIAN_POINT ( 'NONE',  ( -0.1151913129404333325, 0.3392387706403566239, -3.115157480314960647 ) ) ;
#10116 = DIRECTION ( 'NONE',  ( 0.000000000000000000, 1.000000000000000000, 0.000000000000000000 ) ) ;
#10117 = CARTESIAN_POINT ( 'NONE',  ( 0.1522836969735573143, 0.2938892803217901806, -0.3971963147566898167 ) ) ;
#10118 = CARTESIAN_POINT ( 'NONE',  ( -0.09842519685039370636, -0.07874015748031495954, -0.04546065111729338803 ) ) ;
#10119 = DIRECTION ( 'NONE',  ( 1.000000000000000000, 7.017815999999999636E-18, 0.000000000000000000 ) ) ;
#10120 = VECTOR ( 'NONE', #15252, 39.37007874015748854 ) ;
#10121 = CARTESIAN_POINT ( 'NONE',  ( 0.000000000000000000, 0.000000000000000000, 0.1322834645669291320 ) ) ;
#10122 = ORIENTED_EDGE ( 'NONE', *, *, #5150, .F. ) ;
#10123 = DIRECTION ( 'NONE',  ( 0.000000000000000000, 1.000000000000000000, 0.000000000000000000 ) ) ;
#10124 = DIRECTION ( 'NONE',  ( 0.000000000000000000, 0.000000000000000000, 1.000000000000000000 ) ) ;
#10125 = CYLINDRICAL_SURFACE ( 'NONE', #6305, 0.5905511811023621549 ) ;
#10126 = DIRECTION ( 'NONE',  ( 0.000000000000000000, 1.000000000000000000, 0.000000000000000000 ) ) ;
#10127 = DIRECTION ( 'NONE',  ( -1.000000000000000000, 0.000000000000000000, 0.000000000000000000 ) ) ;
#10128 = CARTESIAN_POINT ( 'NONE',  ( 0.2663596103035382745, -0.4612490782035122416, 1.747047244094488194 ) ) ;
#10129 = CARTESIAN_POINT ( 'NONE',  ( 0.3988311005572732215, 0.4763376377695315300, 0.2574803149606298969 ) ) ;
#10130 = CARTESIAN_POINT ( 'NONE',  ( 0.5085118447801136865, 0.06699507805368522251, 1.747047244094488194 ) ) ;
#10131 = ORIENTED_EDGE ( 'NONE', *, *, #22612, .F. ) ;
#10132 = EDGE_CURVE ( 'NONE', #1951, #5345, #15063, .T. ) ;
#10133 = CARTESIAN_POINT ( 'NONE',  ( -0.4165721057576322606, 0.3313508221749649763, 0.1322834645669291320 ) ) ;
#10134 = VERTEX_POINT ( 'NONE', #6113 ) ;
#10135 = CARTESIAN_POINT ( 'NONE',  ( 0.4465874321618643061, -0.1200170377978880404, -1.928289503579156960 ) ) ;
#10136 = CARTESIAN_POINT ( 'NONE',  ( 0.1501355178992943018, -0.4826710871606547104, 0.03296692058226987493 ) ) ;
#10137 = CARTESIAN_POINT ( 'NONE',  ( 0.2211428102655695338, -0.2521176338356630464, 1.973425196850393970 ) ) ;
#10138 = ORIENTED_EDGE ( 'NONE', *, *, #13111, .F. ) ;
#10139 = CARTESIAN_POINT ( 'NONE',  ( 0.06441834428465775808, -0.4889536969034878333, -1.550196850393700920 ) ) ;
#10140 = CIRCLE ( 'NONE', #27761, 0.6299212598425196763 ) ;
#10141 = VERTEX_POINT ( 'NONE', #8363 ) ;
#10142 = ORIENTED_EDGE ( 'NONE', *, *, #9857, .T. ) ;
#10143 = VERTEX_POINT ( 'NONE', #5683 ) ;
#10144 = CONTEXT_DEPENDENT_SHAPE_REPRESENTATION ( #5087, #9591 ) ;
#10145 = DIRECTION ( 'NONE',  ( 0.000000000000000000, 1.000000000000000000, 0.000000000000000000 ) ) ;
#10146 = DIRECTION ( 'NONE',  ( -1.000000000000000000, 0.000000000000000000, 0.000000000000000000 ) ) ;
#10147 = DIRECTION ( 'NONE',  ( 0.000000000000000000, 1.000000000000000000, 0.000000000000000000 ) ) ;
#10148 = CIRCLE ( 'NONE', #25491, 0.2952755905264887182 ) ;
#10149 = ORIENTED_EDGE ( 'NONE', *, *, #19269, .T. ) ;
#10150 = CARTESIAN_POINT ( 'NONE',  ( -0.3217486617182078734, 0.3837523410419874659, 0.2574827755769819038 ) ) ;
#10151 = CARTESIAN_POINT ( 'NONE',  ( -0.1447526197146041249, -0.3977045540727763839, 0.2145688976377952695 ) ) ;
#10152 = CARTESIAN_POINT ( 'NONE',  ( 3.387491338582676492E-16, -0.6299212598425195653, 0.5915354330708662012 ) ) ;
#10153 = AXIS2_PLACEMENT_3D ( 'NONE', #4817, #465, #23649 ) ;
#10154 = VECTOR ( 'NONE', #20507, 39.37007874015748143 ) ;
#10155 = CARTESIAN_POINT ( 'NONE',  ( 0.3543307086614173040, -1.934043700787401319E-18, 0.000000000000000000 ) ) ;
#10156 = CARTESIAN_POINT ( 'NONE',  ( 0.000000000000000000, 0.9055118110236221041, 0.000000000000000000 ) ) ;
#10157 = EDGE_CURVE ( 'NONE', #24360, #22680, #18939, .T. ) ;
#10158 = ORIENTED_EDGE ( 'NONE', *, *, #19573, .T. ) ;
#10159 = VERTEX_POINT ( 'NONE', #18648 ) ;
#10160 = ADVANCED_FACE ( 'NONE', ( #5824 ), #3680, .F. ) ;
#10161 = VECTOR ( 'NONE', #14029, 39.37007874015748854 ) ;
#10162 = ORIENTED_EDGE ( 'NONE', *, *, #9292, .T. ) ;
#10163 = DIRECTION ( 'NONE',  ( 1.000000000000000000, 0.000000000000000000, 0.000000000000000000 ) ) ;
#10164 = EDGE_CURVE ( 'NONE', #5599, #607, #5966, .T. ) ;
#10165 = CARTESIAN_POINT ( 'NONE',  ( 6.147461752294700483E-18, 0.5610236220472440971, 0.2775610236220472093 ) ) ;
#10166 = DIRECTION ( 'NONE',  ( 0.000000000000000000, 0.000000000000000000, 1.000000000000000000 ) ) ;
#10167 = ORIENTED_EDGE ( 'NONE', *, *, #14778, .F. ) ;
#10168 = ORIENTED_EDGE ( 'NONE', *, *, #19797, .F. ) ;
#10169 = CARTESIAN_POINT ( 'NONE',  ( 0.5378903297326614874, 0.4292762795476984805, 0.3401599409343964431 ) ) ;
#10170 = CIRCLE ( 'NONE', #23299, 0.4692913385826771866 ) ;
#10171 = FACE_OUTER_BOUND ( 'NONE', #10325, .T. ) ;
#10172 = DIRECTION ( 'NONE',  ( 0.000000000000000000, 1.000000000000000000, 0.000000000000000000 ) ) ;
#10173 = CARTESIAN_POINT ( 'NONE',  ( -0.09842519685039385902, 0.2165354330708661457, -3.548228346456693050 ) ) ;
#10174 = ORIENTED_EDGE ( 'NONE', *, *, #18912, .T. ) ;
#10175 = CARTESIAN_POINT ( 'NONE',  ( 0.0006679551606482677165, 0.5322830454629158270, 0.1322834645669291320 ) ) ;
#10176 = CARTESIAN_POINT ( 'NONE',  ( 0.3122781343789127195, -0.4068940122751822930, -1.550196850393700476 ) ) ;
#10177 = ORIENTED_EDGE ( 'NONE', *, *, #14019, .F. ) ;
#10178 = CARTESIAN_POINT ( 'NONE',  ( 0.2211428102655656758, 0.2521176338356670432, 1.953740157480315043 ) ) ;
#10179 = CARTESIAN_POINT ( 'NONE',  ( 0.4069448477569521661, 0.3121994997578569353, -1.550196850393700920 ) ) ;
#10180 = ADVANCED_FACE ( 'NONE', ( #7938 ), #27577, .T. ) ;
#10181 = DIRECTION ( 'NONE',  ( -1.000000000000000000, 0.000000000000000000, 0.000000000000000000 ) ) ;
#10182 = CARTESIAN_POINT ( 'NONE',  ( 0.1775991818008583745, 0.5230301363771922007, 0.9399606299212598381 ) ) ;
#10183 = CARTESIAN_POINT ( 'NONE',  ( 0.000000000000000000, 0.000000000000000000, 0.3401574803149606252 ) ) ;
#10184 = FACE_BOUND ( 'NONE', #16326, .T. ) ;
#10185 = EDGE_LOOP ( 'NONE', ( #12804, #5582 ) ) ;
#10186 = CARTESIAN_POINT ( 'NONE',  ( 0.4930758245789425009, 0.08754571829529310401, 0.09685039370078740717 ) ) ;
#10187 = CARTESIAN_POINT ( 'NONE',  ( 1.692913385826771533, 0.4724409448818898127, -0.1181102362204716899 ) ) ;
#10188 = CIRCLE ( 'NONE', #21950, 0.05216535433070866590 ) ;
#10189 = EDGE_CURVE ( 'NONE', #3293, #21048, #1053, .T. ) ;
#10190 = EDGE_LOOP ( 'NONE', ( #17326, #18059, #7909, #21996 ) ) ;
#10191 = CIRCLE ( 'NONE', #20579, 0.7539370078740157410 ) ;
#10192 = EDGE_LOOP ( 'NONE', ( #18703, #16641, #2309, #12533, #10236, #25887 ) ) ;
#10193 = CARTESIAN_POINT ( 'NONE',  ( -2.273123186440590970, -0.6468501409757874132, 1.633858267716535639 ) ) ;
#10194 = EDGE_CURVE ( 'NONE', #6124, #5913, #14842, .T. ) ;
#10195 = DIRECTION ( 'NONE',  ( 0.000000000000000000, 0.000000000000000000, -1.000000000000000000 ) ) ;
#10196 = DIRECTION ( 'NONE',  ( 0.000000000000000000, 0.000000000000000000, 1.000000000000000000 ) ) ;
#10197 = CARTESIAN_POINT ( 'NONE',  ( 0.4004902621173889732, -0.3511566718594057446, 1.747047244094488416 ) ) ;
#10198 = CARTESIAN_POINT ( 'NONE',  ( -0.2268967137093978459, 0.4599980997182848141, -1.550196850393700476 ) ) ;
#10199 = ORIENTED_EDGE ( 'NONE', *, *, #26539, .T. ) ;
#10200 = CARTESIAN_POINT ( 'NONE',  ( -0.5608505875055256329, -0.5625442442700501200, 0.9710808210050355660 ) ) ;
#10201 = VERTEX_POINT ( 'NONE', #14597 ) ;
#10202 = CARTESIAN_POINT ( 'NONE',  ( -0.6003336567877981533, -0.5548708040260077468, -0.9753554781213541469 ) ) ;
#10203 = CARTESIAN_POINT ( 'NONE',  ( -0.5634519861469524660, -0.5309697779850665045, -0.9857434533500372131 ) ) ;
#10204 = DIRECTION ( 'NONE',  ( -1.000000000000000000, 0.000000000000000000, 0.000000000000000000 ) ) ;
#10205 = CARTESIAN_POINT ( 'NONE',  ( -0.1181102362204724532, 0.000000000000000000, 0.6228346456772185791 ) ) ;
#10206 = FACE_OUTER_BOUND ( 'NONE', #13779, .T. ) ;
#10207 = EDGE_LOOP ( 'NONE', ( #12640, #5563, #7550, #10492 ) ) ;
#10208 = EDGE_CURVE ( 'NONE', #24768, #19774, #3280, .T. ) ;
#10209 = DIRECTION ( 'NONE',  ( 0.000000000000000000, -1.000000000000000000, 0.000000000000000000 ) ) ;
#10210 = EDGE_LOOP ( 'NONE', ( #16575, #7286, #13502, #17625 ) ) ;
#10211 = DIRECTION ( 'NONE',  ( -1.000000000000000000, 0.000000000000000000, 0.000000000000000000 ) ) ;
#10212 = CIRCLE ( 'NONE', #24643, 0.08582677165167480748 ) ;
#10213 = ORIENTED_EDGE ( 'NONE', *, *, #11996, .T. ) ;
#10214 = CARTESIAN_POINT ( 'NONE',  ( 0.09275248786854008165, -0.3460502918090608282, -3.115157480314960647 ) ) ;
#10215 = DIRECTION ( 'NONE',  ( 0.4999999999999998890, 0.8660254037844388186, 0.000000000000000000 ) ) ;
#10216 = EDGE_LOOP ( 'NONE', ( #20135, #5151 ) ) ;
#10217 = CARTESIAN_POINT ( 'NONE',  ( -0.2268989272875881757, -0.3929158813954942153, -1.934055118110236338 ) ) ;
#10218 = AXIS2_PLACEMENT_3D ( 'NONE', #24343, #22790, #5123 ) ;
#10219 = B_SPLINE_CURVE_WITH_KNOTS ( 'NONE', 3,
 ( #12277, #21184, #10150, #18765, #23171, #3805 ),
 .UNSPECIFIED., .F., .F.,
 ( 4, 2, 4 ),
 ( 0.9031406754215579591, 0.9046454396443720514, 0.9061502038671860326 ),
 .UNSPECIFIED. ) ;
#10220 = EDGE_LOOP ( 'NONE', ( #1456, #18311, #26489, #5810, #25153, #21984 ) ) ;
#10221 = VERTEX_POINT ( 'NONE', #23060 ) ;
#10222 = CARTESIAN_POINT ( 'NONE',  ( -0.5172021183779732523, -0.4363830659385236621, -0.008640819949054292723 ) ) ;
#10223 = ( CONVERSION_BASED_UNIT ( 'INCH', #18990 ) LENGTH_UNIT ( ) NAMED_UNIT ( #6195 ) ) ;
#10224 = CARTESIAN_POINT ( 'NONE',  ( -0.1712563538833044852, 0.5043504886477827576, 1.747047244094488194 ) ) ;
#10225 = EDGE_CURVE ( 'NONE', #10260, #20147, #16388, .T. ) ;
#10226 = ( NAMED_UNIT ( * ) SI_UNIT ( $, .STERADIAN. ) SOLID_ANGLE_UNIT ( ) ) ;
#10227 = ORIENTED_EDGE ( 'NONE', *, *, #21558, .F. ) ;
#10228 = CARTESIAN_POINT ( 'NONE',  ( 0.000000000000000000, 0.000000000000000000, 0.6299212598425196763 ) ) ;
#10229 = VECTOR ( 'NONE', #22467, 39.37007874015748143 ) ;
#10230 = CARTESIAN_POINT ( 'NONE',  ( 0.2092582568855835823, -0.4359957531126701924, 0.2008762816647728100 ) ) ;
#10231 = PRODUCT ( 'Shaft Seal 20x35x7', 'Shaft Seal 20x35x7', '', ( #6055 ) ) ;
#10232 = CARTESIAN_POINT ( 'NONE',  ( 0.2268599607420258568, -0.6212949646986238861, 0.1926811207639263224 ) ) ;
#10233 = ADVANCED_FACE ( 'NONE', ( #1572 ), #4173, .T. ) ;
#10234 = CARTESIAN_POINT ( 'NONE',  ( 0.2161381151963039093, -0.2817310484609168442, 1.953740157480315043 ) ) ;
#10235 = ORIENTED_EDGE ( 'NONE', *, *, #27618, .F. ) ;
#10236 = ORIENTED_EDGE ( 'NONE', *, *, #11293, .T. ) ;
#10237 = CARTESIAN_POINT ( 'NONE',  ( -0.6562077975700374433, -1.365924015748031427E-17, -0.2362204724409449064 ) ) ;
#10239 = CARTESIAN_POINT ( 'NONE',  ( 0.1429116519061152946, -0.5335524835331961757, 0.9399606299212598381 ) ) ;
#10238 = CARTESIAN_POINT ( 'NONE',  ( -0.3606190329934327310, 0.4297690281277732338, 0.2775610236220472093 ) ) ;
#10240 = ORIENTED_EDGE ( 'NONE', *, *, #15648, .F. ) ;
#10241 = ORIENTED_EDGE ( 'NONE', *, *, #8485, .F. ) ;
#10242 = DIRECTION ( 'NONE',  ( 0.000000000000000000, -1.000000000000000000, 0.000000000000000000 ) ) ;
#10243 = DIRECTION ( 'NONE',  ( 0.000000000000000000, -1.000000000000000000, 0.000000000000000000 ) ) ;
#10244 = CARTESIAN_POINT ( 'NONE',  ( 0.3460635936745020680, -0.09269288654273737105, -3.115157480314960647 ) ) ;
#10245 = CARTESIAN_POINT ( 'NONE',  ( 0.4407612517155324316, -0.3387265385688509323, 0.9202755905511812440 ) ) ;
#10246 = DIRECTION ( 'NONE',  ( 0.000000000000000000, 0.000000000000000000, -1.000000000000000000 ) ) ;
#10247 = CARTESIAN_POINT ( 'NONE',  ( -0.3722026523000413478, 0.000000000000000000, -0.1309055118110236116 ) ) ;
#10248 = CARTESIAN_POINT ( 'NONE',  ( -0.09842519685039370636, 5.809059055118109875E-18, -0.09092130223458683158 ) ) ;
#10249 = TOROIDAL_SURFACE ( 'NONE', #26048, 0.4232283464566928832, 0.07677165354330708902 ) ;
#10250 = DIRECTION ( 'NONE',  ( -0.000000000000000000, -1.000000000000000000, -0.000000000000000000 ) ) ;
#10251 = CARTESIAN_POINT ( 'NONE',  ( 0.7845931698711713365, 0.3318803385907665437, -0.3024313949403425461 ) ) ;
#10252 = CARTESIAN_POINT ( 'NONE',  ( 0.3209354104564642318, 0.3834063931595186880, 0.1259302777253356043 ) ) ;
#10253 = ( GEOMETRIC_REPRESENTATION_CONTEXT ( 3 ) GLOBAL_UNCERTAINTY_ASSIGNED_CONTEXT ( ( #26832 ) ) GLOBAL_UNIT_ASSIGNED_CONTEXT ( ( #24681, #20168, #18602 ) ) REPRESENTATION_CONTEXT ( 'NONE', 'WORKASPACE' ) ) ;
#10254 = DIRECTION ( 'NONE',  ( 1.000000000000000000, 0.000000000000000000, 0.000000000000000000 ) ) ;
#10255 = AXIS2_PLACEMENT_3D ( 'NONE', #17455, #2062, #10673 ) ;
#10256 = VERTEX_POINT ( 'NONE', #22751 ) ;
#10257 = CARTESIAN_POINT ( 'NONE',  ( 0.1481194149833036655, 0.5525858403826197085, 0.9399606299212600602 ) ) ;
#10258 = ADVANCED_FACE ( 'NONE', ( #16528 ), #27846, .T. ) ;
#10259 = DIRECTION ( 'NONE',  ( 1.000000000000000000, 0.000000000000000000, 0.000000000000000000 ) ) ;
#10260 = VERTEX_POINT ( 'NONE', #27707 ) ;
#10261 = DIRECTION ( 'NONE',  ( 1.000000000000000000, 0.000000000000000000, 0.000000000000000000 ) ) ;
#10262 = CARTESIAN_POINT ( 'NONE',  ( 0.000000000000000000, 0.2952755905511810774, 0.2637795275590551491 ) ) ;
#10263 = CARTESIAN_POINT ( 'NONE',  ( -0.3169330146478837040, -0.1835719822040729754, 0.08455817587859276729 ) ) ;
#10264 = EDGE_CURVE ( 'NONE', #3934, #24215, #2794, .T. ) ;
#10265 = CARTESIAN_POINT ( 'NONE',  ( -0.4069448477556103505, 0.3121994997598293020, 1.766732283464566899 ) ) ;
#10266 = VERTEX_POINT ( 'NONE', #12713 ) ;
#10267 = EDGE_CURVE ( 'NONE', #20711, #15905, #5523, .T. ) ;
#10268 = VERTEX_POINT ( 'NONE', #18639 ) ;
#10269 = DIRECTION ( 'NONE',  ( 1.000000000000000000, 0.000000000000000000, 0.000000000000000000 ) ) ;
#10270 = VERTEX_POINT ( 'NONE', #27276 ) ;
#10271 = CARTESIAN_POINT ( 'NONE',  ( 0.3924375359088155268, 0.3121297331100029715, 0.1643955689165516598 ) ) ;
#10272 = CARTESIAN_POINT ( 'NONE',  ( -0.4233199042382427835, 0.5034331896112764770, 0.2081850588231654031 ) ) ;
#10273 = CARTESIAN_POINT ( 'NONE',  ( -0.4446020952038907681, 0.02909913904661337244, -1.934055118110236338 ) ) ;
#10274 = CARTESIAN_POINT ( 'NONE',  ( 0.1490609433494345937, -0.4786070381568061083, 0.009463581268761192544 ) ) ;
#10275 = AXIS2_PLACEMENT_3D ( 'NONE', #22450, #18036, #5210 ) ;
#10276 = CARTESIAN_POINT ( 'NONE',  ( 0.02190250779246093876, -0.3346456692913385433, 1.973425196850393970 ) ) ;
#10277 = VERTEX_POINT ( 'NONE', #23048 ) ;
#10278 = CARTESIAN_POINT ( 'NONE',  ( -0.4270824798167728864, 0.2466292688015120915, -1.550196850393700920 ) ) ;
#10279 = CARTESIAN_POINT ( 'NONE',  ( -0.3715251363271980245, 0.06498290224717540031, 0.1992125984251968684 ) ) ;
#10280 = AXIS2_PLACEMENT_3D ( 'NONE', #7582, #813, #22696 ) ;
#10281 = ORIENTED_EDGE ( 'NONE', *, *, #26237, .F. ) ;
#10282 = ORIENTED_EDGE ( 'NONE', *, *, #928, .F. ) ;
#10283 = DIRECTION ( 'NONE',  ( 0.000000000000000000, 0.000000000000000000, -1.000000000000000000 ) ) ;
#10284 = DIRECTION ( 'NONE',  ( 0.7660444431189780135, 0.6427876096865392519, 0.000000000000000000 ) ) ;
#10285 = CARTESIAN_POINT ( 'NONE',  ( 0.000000000000000000, 0.000000000000000000, 0.2637795275590551491 ) ) ;
#10286 = CARTESIAN_POINT ( 'NONE',  ( 0.1658556822987644341, -0.4573967274800467275, 0.2467937633379344575 ) ) ;
#10287 = VERTEX_POINT ( 'NONE', #7929 ) ;
#10288 = FACE_BOUND ( 'NONE', #6924, .T. ) ;
#10289 = VECTOR ( 'NONE', #8596, 39.37007874015748143 ) ;
#10290 = DIRECTION ( 'NONE',  ( 0.000000000000000000, 1.000000000000000000, 0.000000000000000000 ) ) ;
#10291 = DIRECTION ( 'NONE',  ( -1.000000000000000078E-15, 1.000000000000000000, 0.000000000000000000 ) ) ;
#10292 = CARTESIAN_POINT ( 'NONE',  ( -0.5941926817969179764, -0.2205403317192303758, 0.2172113851610799617 ) ) ;
#10293 = AXIS2_PLACEMENT_3D ( 'NONE', #19230, #27862, #25874 ) ;
#10294 = CARTESIAN_POINT ( 'NONE',  ( 0.06002032661671171526, 0.4585215200179057482, -1.928289503579156516 ) ) ;
#10295 = CARTESIAN_POINT ( 'NONE',  ( 0.3070866141732283561, 0.000000000000000000, -1.639108858267716421E-17 ) ) ;
#10296 = ADVANCED_FACE ( 'NONE', ( #12295 ), #25602, .T. ) ;
#10297 = TOROIDAL_SURFACE ( 'NONE', #12119, 0.4232283464566928832, 0.07677165354330708902 ) ;
#10298 = CARTESIAN_POINT ( 'NONE',  ( -0.4793172621399190425, 0.1288129352161815067, -1.569881889763779625 ) ) ;
#10299 = CARTESIAN_POINT ( 'NONE',  ( -0.4405067310592692409, 0.000000000000000000, -0.1627508102905848297 ) ) ;
#10300 = EDGE_CURVE ( 'NONE', #6477, #17148, #19514, .T. ) ;
#10301 = CARTESIAN_POINT ( 'NONE',  ( 0.5383572925355708527, -0.3100567972184350429, 0.2574803149606298969 ) ) ;
#10302 = ORIENTED_EDGE ( 'NONE', *, *, #13330, .T. ) ;
#10303 = ORIENTED_EDGE ( 'NONE', *, *, #17167, .T. ) ;
#10304 = CARTESIAN_POINT ( 'NONE',  ( 0.1589886963210821458, -0.4351482077929094694, 0.2048502515443846317 ) ) ;
#10305 = ORIENTED_EDGE ( 'NONE', *, *, #3152, .T. ) ;
#10306 = EDGE_LOOP ( 'NONE', ( #1383, #7469, #1157, #8979, #9812 ) ) ;
#10307 = CARTESIAN_POINT ( 'NONE',  ( -0.5118110236220763110, -0.03349795313034512750, -1.550196850393700920 ) ) ;
#10308 = CARTESIAN_POINT ( 'NONE',  ( 0.000000000000000000, 0.000000000000000000, 0.1771653543307086520 ) ) ;
#10309 = CARTESIAN_POINT ( 'NONE',  ( 0.1522836969735572310, 0.4941010236220472751, 0.000000000000000000 ) ) ;
#10310 = DIRECTION ( 'NONE',  ( 0.000000000000000000, 0.000000000000000000, -1.000000000000000000 ) ) ;
#10311 = DIMENSIONAL_EXPONENTS ( 1.000000000000000000, 0.000000000000000000, 0.000000000000000000, 0.000000000000000000, 0.000000000000000000, 0.000000000000000000, 0.000000000000000000 ) ;
#10312 = ORIENTED_EDGE ( 'NONE', *, *, #5546, .T. ) ;
#10313 = CARTESIAN_POINT ( 'NONE',  ( 0.000000000000000000, 0.000000000000000000, -0.05856299212598425896 ) ) ;
#10314 = ( CONVERSION_BASED_UNIT ( 'INCH', #18499 ) LENGTH_UNIT ( ) NAMED_UNIT ( #10500 ) ) ;
#10315 = CIRCLE ( 'NONE', #16642, 0.5322834645669292097 ) ;
#10316 = AXIS2_PLACEMENT_3D ( 'NONE', #24959, #22999, #5618 ) ;
#10317 = CARTESIAN_POINT ( 'NONE',  ( 0.000000000000000000, 0.5322834645669292097, 0.3401599409343964431 ) ) ;
#10318 = DIRECTION ( 'NONE',  ( 1.000000000000000000, 0.000000000000000000, 0.000000000000000000 ) ) ;
#10319 = ADVANCED_FACE ( 'NONE', ( #2463 ), #27189, .T. ) ;
#10320 = EDGE_CURVE ( 'NONE', #24998, #13907, #377, .T. ) ;
#10321 = CARTESIAN_POINT ( 'NONE',  ( -0.1714649452450071054, -0.4705186852026070898, 0.2574827755769819038 ) ) ;
#10322 = ORIENTED_EDGE ( 'NONE', *, *, #22177, .T. ) ;
#10323 = CARTESIAN_POINT ( 'NONE',  ( -0.4010740433761567081, 0.000000000000000000, -0.2342519685039370358 ) ) ;
#10324 = PRODUCT_DEFINITION ( 'UNKNOWN', '', #13832, #8531 ) ;
#10325 = EDGE_LOOP ( 'NONE', ( #17826, #11809, #8130, #21397, #27271 ) ) ;
#10326 = AXIS2_PLACEMENT_3D ( 'NONE', #24650, #22832, #7721 ) ;
#10327 = CARTESIAN_POINT ( 'NONE',  ( 0.1078280746903962500, -0.3175540113612315696, 1.973425196850393970 ) ) ;
#10328 = LINE ( 'NONE', #12164, #445 ) ;
#10329 = CARTESIAN_POINT ( 'NONE',  ( 0.000000000000000000, 0.000000000000000000, -0.1756889763779527769 ) ) ;
#10330 = AXIS2_PLACEMENT_3D ( 'NONE', #8904, #8630, #4662 ) ;
#10331 = CARTESIAN_POINT ( 'NONE',  ( -0.3362148458988341582, -0.4382482975805541692, 0.9399606299212598381 ) ) ;
#10332 = ADVANCED_FACE ( 'NONE', ( #26063 ), #13970, .T. ) ;
#10333 = EDGE_CURVE ( 'NONE', #3752, #2655, #7053, .T. ) ;
#10334 = SPHERICAL_SURFACE ( 'NONE', #24090, 0.1003956692913385851 ) ;
#10335 = VERTEX_POINT ( 'NONE', #3633 ) ;
#10336 = DIRECTION ( 'NONE',  ( 0.000000000000000000, 0.000000000000000000, 1.000000000000000000 ) ) ;
#10337 = PLANE ( 'NONE',  #27093 ) ;
#10338 = AXIS2_PLACEMENT_3D ( 'NONE', #19787, #11303, #21638 ) ;
#10339 = ( REPRESENTATION_RELATIONSHIP ('NONE','NONE', #12434, #16232 ) REPRESENTATION_RELATIONSHIP_WITH_TRANSFORMATION ( #25124 )SHAPE_REPRESENTATION_RELATIONSHIP( ) ) ;
#10340 = AXIS2_PLACEMENT_3D ( 'NONE', #19656, #4661, #19506 ) ;
#10341 = CARTESIAN_POINT ( 'NONE',  ( -0.2356229156547619552, 0.4776874499716828870, 1.747047244094488416 ) ) ;
#10342 = ORIENTED_EDGE ( 'NONE', *, *, #10985, .T. ) ;
#10343 = CARTESIAN_POINT ( 'NONE',  ( 0.4954415918535723939, -0.1327036767636087800, -1.550196850393700920 ) ) ;
#10344 = DIRECTION ( 'NONE',  ( 0.000000000000000000, 0.000000000000000000, 1.000000000000000000 ) ) ;
#10345 = DIRECTION ( 'NONE',  ( 0.000000000000000000, 0.000000000000000000, -1.000000000000000000 ) ) ;
#10346 = CARTESIAN_POINT ( 'NONE',  ( -0.1285103288269285327, -0.3545966721392122545, 0.1992125984251968684 ) ) ;
#10347 = CARTESIAN_POINT ( 'NONE',  ( 0.4613022222206614176, -0.2662775206743260847, 1.747047244094488194 ) ) ;
#10348 = ORIENTED_EDGE ( 'NONE', *, *, #19068, .T. ) ;
#10349 = CARTESIAN_POINT ( 'NONE',  ( -0.5819142500240400695, -0.6280845039713092159, 0.9045795100218007034 ) ) ;
#10350 = VERTEX_POINT ( 'NONE', #22871 ) ;
#10351 = CARTESIAN_POINT ( 'NONE',  ( -0.6098677386912745302, -0.5016113632408703005, -0.9930866184834644672 ) ) ;
#10352 = DIRECTION ( 'NONE',  ( 0.000000000000000000, 0.000000000000000000, 1.000000000000000000 ) ) ;
#10353 = DIRECTION ( 'NONE',  ( 1.224646799147353207E-16, 1.000000000000000000, -0.000000000000000000 ) ) ;
#10354 = CARTESIAN_POINT ( 'NONE',  ( 0.1658689444481890873, -0.4574452598415587601, 0.1827409795207127485 ) ) ;
#10355 = AXIS2_PLACEMENT_3D ( 'NONE', #4651, #13277, #14875 ) ;
#10356 = CARTESIAN_POINT ( 'NONE',  ( 8.741913385826771462E-17, 0.1673228346456692994, 0.000000000000000000 ) ) ;
#10357 = EDGE_CURVE ( 'NONE', #17040, #3411, #17791, .T. ) ;
#10358 = B_SPLINE_CURVE_WITH_KNOTS ( 'NONE', 3,
 ( #10777, #19805, #25758, #15175, #467, #4427 ),
 .UNSPECIFIED., .F., .F.,
 ( 4, 2, 4 ),
 ( 0.4045103800602309896, 0.4064350009536160102, 0.4083596218470010308 ),
 .UNSPECIFIED. ) ;
#10359 = AXIS2_PLACEMENT_3D ( 'NONE', #6590, #6445, #12931 ) ;
#10360 = CARTESIAN_POINT ( 'NONE',  ( 0.1490609433615242285, 0.4786070381542913421, 0.000000000000000000 ) ) ;
#10361 = EDGE_CURVE ( 'NONE', #4142, #8364, #25358, .T. ) ;
#10362 = ORIENTED_EDGE ( 'NONE', *, *, #19686, .F. ) ;
#10363 = ADVANCED_FACE ( 'NONE', ( #12121, #16229 ), #5919, .T. ) ;
#10364 = CARTESIAN_POINT ( 'NONE',  ( -0.4069519308876702324, -0.2006393256663696334, -1.934055118110236338 ) ) ;
#10365 = EDGE_CURVE ( 'NONE', #783, #20567, #26963, .T. ) ;
#10366 = VERTEX_POINT ( 'NONE', #27107 ) ;
#10367 = VERTEX_POINT ( 'NONE', #16368 ) ;
#10368 = CARTESIAN_POINT ( 'NONE',  ( -0.5743180011325290657, -0.2193631536940708893, -0.1036282081129438898 ) ) ;
#10369 = CARTESIAN_POINT ( 'NONE',  ( 0.1918813796216842782, -0.5271897577243779276, 0.1771653543307086520 ) ) ;
#10370 = CARTESIAN_POINT ( 'NONE',  ( 0.2355331214654129424, 0.4777261797697872625, 1.747047244094488194 ) ) ;
#10371 = EDGE_LOOP ( 'NONE', ( #19536, #17742, #7363, #16897 ) ) ;
#10372 = CIRCLE ( 'NONE', #3139, 0.07677362204724411110 ) ;
#10373 = ORIENTED_EDGE ( 'NONE', *, *, #1565, .F. ) ;
#10374 = AXIS2_PLACEMENT_3D ( 'NONE', #27120, #24982, #25270 ) ;
#10375 = CARTESIAN_POINT ( 'NONE',  ( -0.3661417322834645272, -0.4724409448818898127, 0.8182917201112815953 ) ) ;
#10376 = DIRECTION ( 'NONE',  ( 0.000000000000000000, 0.000000000000000000, 1.000000000000000000 ) ) ;
#10377 = CARTESIAN_POINT ( 'NONE',  ( -0.09842519685039370636, 0.07874015748031495954, 0.04546065111729331171 ) ) ;
#10378 = CARTESIAN_POINT ( 'NONE',  ( 0.1153557615288998417, 0.4303681241740018315, -1.934055118110236116 ) ) ;
#10379 = ORIENTED_EDGE ( 'NONE', *, *, #21049, .T. ) ;
#10380 = CARTESIAN_POINT ( 'NONE',  ( -0.3429980251342297226, 0.09187177619658862260, 1.953740157480315043 ) ) ;
#10381 = VERTEX_POINT ( 'NONE', #1385 ) ;
#10382 = AXIS2_PLACEMENT_3D ( 'NONE', #4043, #20987, #3894 ) ;
#10383 = CARTESIAN_POINT ( 'NONE',  ( -0.5098050478186216816, -0.3322734260891199165, -0.3067987715593742948 ) ) ;
#10385 = CARTESIAN_POINT ( 'NONE',  ( 0.4300830224589536899, -0.3772436174784755680, 0.9399606299212598381 ) ) ;
#10384 = CARTESIAN_POINT ( 'NONE',  ( 0.4062254136079196942, -0.2349793847445169337, 0.1992142434433712694 ) ) ;
#10386 = CARTESIAN_POINT ( 'NONE',  ( -1.692913385826771533, 0.07874015748031495954, 0.1181102362204718981 ) ) ;
#10387 = ORIENTED_EDGE ( 'NONE', *, *, #15270, .T. ) ;
#10388 = VERTEX_POINT ( 'NONE', #27530 ) ;
#10389 = CYLINDRICAL_SURFACE ( 'NONE', #6702, 0.7874015748208159637 ) ;
#10390 = CARTESIAN_POINT ( 'NONE',  ( -0.5112608635011182123, 0.4023796438212055016, -0.1315133041178671303 ) ) ;
#10391 = EDGE_CURVE ( 'NONE', #15450, #13929, #9613, .T. ) ;
#10392 = ( BOUNDED_CURVE ( )  B_SPLINE_CURVE ( 2, ( #19344, #21192, #23036 ),
 .UNSPECIFIED., .F., .T. ) 
 B_SPLINE_CURVE_WITH_KNOTS ( ( 3, 3 ),
 ( 0.000000000000000000, 0.2336872276155829986 ),
 .UNSPECIFIED. ) 
 CURVE ( )  GEOMETRIC_REPRESENTATION_ITEM ( )  RATIONAL_B_SPLINE_CURVE ( ( 1.000000000000000000, 1.154700538379251906, 1.000000000000000000 ) ) 
 REPRESENTATION_ITEM ( '' )  ) ;
#10393 = CARTESIAN_POINT ( 'NONE',  ( 0.09269288654274054906, 0.3460635936744927976, -3.115157480314960647 ) ) ;
#10394 = LINE ( 'NONE', #16617, #20684 ) ;
#10395 = DIRECTION ( 'NONE',  ( 0.000000000000000000, -1.000000000000000000, 0.000000000000000000 ) ) ;
#10396 = DIRECTION ( 'NONE',  ( 1.000000000000000000, 0.000000000000000000, 0.000000000000000000 ) ) ;
#10397 = ADVANCED_FACE ( 'NONE', ( #18318 ), #27632, .T. ) ;
#10398 = B_SPLINE_CURVE_WITH_KNOTS ( 'NONE', 3,
 ( #11987, #3786, #12406, #12259, #10002, #14405 ),
 .UNSPECIFIED., .F., .F.,
 ( 4, 2, 4 ),
 ( 0.000000000000000000, 0.5000000000000000000, 1.000000000000000000 ),
 .UNSPECIFIED. ) ;
#10399 = CIRCLE ( 'NONE', #13106, 0.07677362204724411110 ) ;
#10400 = CARTESIAN_POINT ( 'NONE',  ( 0.03532354024591839031, -0.6299212598425196763, 0.000000000000000000 ) ) ;
#10401 = ORIENTED_EDGE ( 'NONE', *, *, #6361, .T. ) ;
#10402 = CYLINDRICAL_SURFACE ( 'NONE', #27867, 0.7874015748208159637 ) ;
#10403 = CARTESIAN_POINT ( 'NONE',  ( 0.000000000000000000, 0.000000000000000000, 0.2637795275590551491 ) ) ;
#10404 = DIRECTION ( 'NONE',  ( 1.000000000000000000, 0.000000000000000000, 0.000000000000000000 ) ) ;
#10405 = ORIENTED_EDGE ( 'NONE', *, *, #2278, .F. ) ;
#10406 = ORIENTED_EDGE ( 'NONE', *, *, #3422, .T. ) ;
#10407 = LINE ( 'NONE', #17191, #9681 ) ;
#10408 = CARTESIAN_POINT ( 'NONE',  ( 0.4777261797697372470, -0.2355331214654103889, 1.747047244094488194 ) ) ;
#10409 = APPLICATION_PROTOCOL_DEFINITION ( 'draft international standard', 'automotive_design', 1998, #17718 ) ;
#10410 = CARTESIAN_POINT ( 'NONE',  ( -0.2268599607415389408, -0.6212949646972618645, 0.1616495878881323567 ) ) ;
#10411 = ORIENTED_EDGE ( 'NONE', *, *, #2229, .F. ) ;
#10412 = EDGE_LOOP ( 'NONE', ( #19833, #923, #11295, #20248 ) ) ;
#10413 = CARTESIAN_POINT ( 'NONE',  ( 0.3574975638436101444, -0.02339816079119092299, -3.115157480314960647 ) ) ;
#10414 = CARTESIAN_POINT ( 'NONE',  ( -0.4006498629591503935, -0.2309201403895324023, -1.928289503579156516 ) ) ;
#10415 = FACE_OUTER_BOUND ( 'NONE', #26359, .T. ) ;
#10416 = CARTESIAN_POINT ( 'NONE',  ( -0.02190250779246035590, 0.3346456692913385988, 1.973425196850393970 ) ) ;
#10417 = ORIENTED_EDGE ( 'NONE', *, *, #23604, .T. ) ;
#10418 = ORIENTED_EDGE ( 'NONE', *, *, #11791, .F. ) ;
#10419 = AXIS2_PLACEMENT_3D ( 'NONE', #5132, #7401, #20254 ) ;
#10420 = CARTESIAN_POINT ( 'NONE',  ( 0.3252100150720097504, 0.3707612262533033776, -1.550196850393700920 ) ) ;
#10421 = CARTESIAN_POINT ( 'NONE',  ( -0.1968503937007874127, 0.9448818897637796255, 0.1082677165354330451 ) ) ;
#10422 = CARTESIAN_POINT ( 'NONE',  ( -0.5511811023622048555, 0.000000000000000000, 0.9399606299212598381 ) ) ;
#10423 = ORIENTED_EDGE ( 'NONE', *, *, #22453, .T. ) ;
#10424 = ORIENTED_EDGE ( 'NONE', *, *, #22013, .T. ) ;
#10425 = AXIS2_PLACEMENT_3D ( 'NONE', #25812, #23965, #4340 ) ;
#10426 = EDGE_CURVE ( 'NONE', #24641, #16499, #10398, .T. ) ;
#10427 = ITEM_DEFINED_TRANSFORMATION ( 'NONE', 'NONE', #27823,  #11588 ) ;
#10428 = CARTESIAN_POINT ( 'NONE',  ( 0.000000000000000000, 0.000000000000000000, -0.2755905511811023723 ) ) ;
#10429 = DIRECTION ( 'NONE',  ( 1.000000000000000000, 0.000000000000000000, 0.000000000000000000 ) ) ;
#10430 = CARTESIAN_POINT ( 'NONE',  ( -1.197070535079588716, 0.07874015748031495954, 1.197070535079588716 ) ) ;
#10431 = ORIENTED_EDGE ( 'NONE', *, *, #4721, .F. ) ;
#10432 = ADVANCED_FACE ( 'NONE', ( #15236 ), #19496, .F. ) ;
#10433 = VERTEX_POINT ( 'NONE', #21721 ) ;
#10434 = CARTESIAN_POINT ( 'NONE',  ( -0.3924375359084866788, 0.3121297331097429018, 0.3080453759647233114 ) ) ;
#10435 = B_SPLINE_CURVE_WITH_KNOTS ( 'NONE', 3,
 ( #3872, #16882, #25626, #6280, #19262, #6691, #604, #9198, #21529, #2439 ),
 .UNSPECIFIED., .F., .F.,
 ( 4, 2, 2, 2, 4 ),
 ( 0.000000000000000000, 0.2500000000000000000, 0.5000000000000000000, 0.7500000000000000000, 1.000000000000000000 ),
 .UNSPECIFIED. ) ;
#10436 = CARTESIAN_POINT ( 'NONE',  ( -0.01968503937007873988, 0.000000000000000000, 0.000000000000000000 ) ) ;
#10437 = CARTESIAN_POINT ( 'NONE',  ( 0.06200787401574805319, 0.000000000000000000, -4.015748031496062964 ) ) ;
#10438 = CARTESIAN_POINT ( 'NONE',  ( 0.8549722296228741136, -0.6488494047548032384, 2.027559055118110187 ) ) ;
#10439 = AXIS2_PLACEMENT_3D ( 'NONE', #17006, #1744, #9162 ) ;
#10440 = CARTESIAN_POINT ( 'NONE',  ( 0.4585215200179055817, -2.840735999735804609E-17, -1.928289503579156516 ) ) ;
#10441 = CARTESIAN_POINT ( 'NONE',  ( 0.2478439864030018702, 0.4300129863948118913, -1.569881889763779625 ) ) ;
#10442 = DIRECTION ( 'NONE',  ( 0.000000000000000000, 0.000000000000000000, -1.000000000000000000 ) ) ;
#10443 = DIMENSIONAL_EXPONENTS ( 1.000000000000000000, 0.000000000000000000, 0.000000000000000000, 0.000000000000000000, 0.000000000000000000, 0.000000000000000000, 0.000000000000000000 ) ;
#10444 = ADVANCED_FACE ( 'NONE', ( #6611 ), #26694, .F. ) ;
#10445 = COLOUR_RGB ( '', 0.31764706, 0.68627451, 0.89019608) ;
#10446 = CARTESIAN_POINT ( 'NONE',  ( 0.4921259842519685179, 0.000000000000000000, -1.934055118110236338 ) ) ;
#10447 = ORIENTED_EDGE ( 'NONE', *, *, #11304, .T. ) ;
#10448 = CARTESIAN_POINT ( 'NONE',  ( -0.08530183727034104657, 0.03937007874015747977, 0.06819097667594015144 ) ) ;
#10449 = EDGE_LOOP ( 'NONE', ( #21860, #13923, #1184, #3638 ) ) ;
#10450 = DIRECTION ( 'NONE',  ( -0.7212949172625979788, 0.000000000000000000, -0.6926280692631088254 ) ) ;
#10451 = CARTESIAN_POINT ( 'NONE',  ( 0.4932136069632150344, 0.08676634416061969335, 0.09684793308443523374 ) ) ;
#10452 = DIRECTION ( 'NONE',  ( 1.000000000000000000, 0.000000000000000000, 0.000000000000000000 ) ) ;
#10453 = CARTESIAN_POINT ( 'NONE',  ( 0.4152525734086276454, 0.3642352168757554964, 0.9202755905511811330 ) ) ;
#10454 = ORIENTED_EDGE ( 'NONE', *, *, #14171, .F. ) ;
#10455 = CARTESIAN_POINT ( 'NONE',  ( -0.3606049308151464960, 0.06410376196625482137, 0.1910323753048591700 ) ) ;
#10456 = CARTESIAN_POINT ( 'NONE',  ( 0.000000000000000000, 0.000000000000000000, 1.747047244094488194 ) ) ;
#10457 = ORIENTED_EDGE ( 'NONE', *, *, #12047, .F. ) ;
#10458 = AXIS2_PLACEMENT_3D ( 'NONE', #27460, #4013, #20958 ) ;
#10459 = CARTESIAN_POINT ( 'NONE',  ( 0.1638952246732497953, -0.5499255957412874096, 6.734645669291338471E-17 ) ) ;
#10460 = CARTESIAN_POINT ( 'NONE',  ( 0.000000000000000000, 0.4232283464566928832, 0.2755905511811023723 ) ) ;
#10461 = EDGE_CURVE ( 'NONE', #16455, #3818, #22200, .T. ) ;
#10462 = DIRECTION ( 'NONE',  ( -1.000000000000000000, 0.000000000000000000, 0.000000000000000000 ) ) ;
#10463 = ORIENTED_EDGE ( 'NONE', *, *, #7468, .T. ) ;
#10464 = CARTESIAN_POINT ( 'NONE',  ( 0.6055690743987126590, -0.2581485381169807414, -0.4471263839182408883 ) ) ;
#10465 = DIRECTION ( 'NONE',  ( -0.000000000000000000, -1.000000000000000000, -0.000000000000000000 ) ) ;
#10466 = EDGE_LOOP ( 'NONE', ( #982, #3793, #3347, #14268, #3214, #4617, #22933, #25259, #23868, #23974, #13954, #20270, #6173 ) ) ;
#10467 = CARTESIAN_POINT ( 'NONE',  ( 0.1078280746903977072, 0.3175540113612247972, 1.953740157480315043 ) ) ;
#10468 = CARTESIAN_POINT ( 'NONE',  ( 0.000000000000000000, 0.000000000000000000, 0.1771653543307086520 ) ) ;
#10469 = CARTESIAN_POINT ( 'NONE',  ( 0.0005789383928842625369, 0.4762008496972124916, 0.2330651857772763624 ) ) ;
#10470 = CARTESIAN_POINT ( 'NONE',  ( 0.4382482975805214731, -0.3362148458988676314, 0.9399606299212598381 ) ) ;
#10471 = LINE ( 'NONE', #27868, #9185 ) ;
#10472 = ORIENTED_EDGE ( 'NONE', *, *, #27640, .T. ) ;
#10473 = B_SPLINE_SURFACE_WITH_KNOTS ( 'NONE', 3, 3, ( 
 ( #20411, #24923, #14213, #27337 ),
 ( #24636, #22392, #15893, #3161 ),
 ( #9815, #22819, #3438, #7848 ),
 ( #20694, #24496, #5448, #3014 ),
 ( #9671, #13920, #18414, #11652 ),
 ( #22535, #18116, #20271, #16040 ),
 ( #12075, #7559, #18554, #9519 ),
 ( #5295, #16184, #22673, #3300 ),
 ( #1210, #1344, #9952, #27199 ),
 ( #16457, #25207, #6164, #18838 ),
 ( #19271, #25774, #21261, #23532 ),
 ( #14647, #1898, #6289, #4165 ),
 ( #19414, #12772, #4303, #25500 ),
 ( #18326, #3881, #6010, #10505 ),
 ( #21398, #23250, #10222, #7988 ),
 ( #12910, #4026, #10796, #23394 ),
 ( #14922, #19128, #12636, #6425 ),
 ( #10651, #27480, #16734, #2039 ),
 ( #1756, #8540, #21115, #23669 ),
 ( #15057, #21535, #17158, #2183 ),
 ( #16594, #10368, #8125, #5873 ),
 ( #25347, #14501, #27762, #23105 ),
 ( #3733, #12356, #18989, #20975 ),
 ( #1618, #27622, #8263, #12500 ),
 ( #16887, #14791, #8405, #17024 ),
 ( #25636, #4701, #8942, #4979 ),
 ( #13595, #10933, #15732, #22217 ),
 ( #6980, #13456, #15467, #17828 ),
 ( #21677, #24204, #2711, #26445 ),
 ( #19824, #2578, #26184, #19554 ),
 ( #236, #485, #17292, #2844 ),
 ( #4569, #24066, #26044, #9206 ),
 ( #13328, #8812, #104, #21811 ),
 ( #11075, #7109, #25914, #24335 ),
 ( #11482, #15187, #8674, #6565 ) ),
 .UNSPECIFIED., .F., .F., .F.,
 ( 4, 1, 1, 1, 1, 1, 1, 1, 1, 1, 1, 1, 1, 1, 1, 1, 1, 1, 1, 1, 1, 1, 1, 1, 1, 1, 1, 1, 1, 1, 1, 1, 4 ),
 ( 4, 4 ),
 ( 1.918259199999999943E-08, 0.04098565352343399443, 0.08197128786427600178, 0.1024641050346969950, 0.1434497393755389816, 0.1639425565459600165, 0.1946817823015919990, 0.2049281908868030022, 0.2254210080572240094, 0.2356674166424339856, 0.2510370295202500324, 0.2561602338128550205, 0.2664066423980660514, 0.2715298466906710395, 0.2817762552758819594, 0.2868994595684870030, 0.2971458681536969793, 0.3022690724463030221, 0.3125154810315129983, 0.3176386853241179864, 0.3278850939093290173, 0.3330082982019340054, 0.3406931046408420150, 0.3432547067871450364, 0.3483779110797499690, 0.3509395132260529904, 0.3560627175186579785, 0.3586243196649609999, 0.3637475239575660435, 0.3663091261038680102, 0.3739939325427759642, 0.3791171368353820070, 0.3833360769390560252 ),
 ( -0.5999999999999999778, 0.5999999999999999778 ),
 .UNSPECIFIED. ) ;
#10474 = CARTESIAN_POINT ( 'NONE',  ( 0.2842139414040969481, 0.2181198385715675259, -3.115157480314960647 ) ) ;
#10475 = AXIS2_PLACEMENT_3D ( 'NONE', #19178, #282, #16785 ) ;
#10476 = CARTESIAN_POINT ( 'NONE',  ( -0.4842519685039370358, 0.000000000000000000, -0.01377952755905511792 ) ) ;
#10477 = ORIENTED_EDGE ( 'NONE', *, *, #16975, .F. ) ;
#10478 = ORIENTED_EDGE ( 'NONE', *, *, #24264, .T. ) ;
#10479 = ADVANCED_FACE ( 'NONE', ( #10415 ), #15460, .T. ) ;
#10480 = CARTESIAN_POINT ( 'NONE',  ( -0.03349795313024159921, 0.5118110236220473341, -1.550196850393700920 ) ) ;
#10481 = CARTESIAN_POINT ( 'NONE',  ( 0.07462095020297215830, -0.5672055940108892136, 0.9399606299212598381 ) ) ;
#10482 = FACE_OUTER_BOUND ( 'NONE', #23618, .T. ) ;
#10483 = DIRECTION ( 'NONE',  ( -0.000000000000000000, -0.000000000000000000, -1.000000000000000000 ) ) ;
#10484 = CARTESIAN_POINT ( 'NONE',  ( -0.4613045817967623696, -0.2662790972929528488, 1.747047244094487972 ) ) ;
#10485 = LINE ( 'NONE', #3556, #21909 ) ;
#10486 = ORIENTED_EDGE ( 'NONE', *, *, #18406, .F. ) ;
#10487 = DIRECTION ( 'NONE',  ( -1.000000000000000000, 0.000000000000000000, 0.000000000000000000 ) ) ;
#10488 = ADVANCED_FACE ( 'NONE', ( #23579, #8721 ), #17342, .T. ) ;
#10489 = CARTESIAN_POINT ( 'NONE',  ( 0.000000000000000000, 0.000000000000000000, 0.04842519685039370358 ) ) ;
#10490 = CARTESIAN_POINT ( 'NONE',  ( 8.741913385826771462E-17, -4.420669291338583154E-18, 0.000000000000000000 ) ) ;
#10491 = CARTESIAN_POINT ( 'NONE',  ( 0.1704479274145334344, -0.4700505334969884430, 0.1259302777270377427 ) ) ;
#10492 = ORIENTED_EDGE ( 'NONE', *, *, #4983, .F. ) ;
#10493 = CIRCLE ( 'NONE', #2811, 0.01377952755905510404 ) ;
#10494 = CARTESIAN_POINT ( 'NONE',  ( 0.3713448905834433322, 0.06600512665679410251, 0.1992125984251968684 ) ) ;
#10495 = CIRCLE ( 'NONE', #25384, 0.2938622683360631593 ) ;
#10496 = CARTESIAN_POINT ( 'NONE',  ( 0.5375739373539409893, 0.4296723508511047229, 0.1322834645669291320 ) ) ;
#10497 = ORIENTED_EDGE ( 'NONE', *, *, #19993, .T. ) ;
#10498 = ORIENTED_EDGE ( 'NONE', *, *, #4673, .T. ) ;
#10499 = VECTOR ( 'NONE', #26354, 39.37007874015748143 ) ;
#10500 = DIMENSIONAL_EXPONENTS ( 1.000000000000000000, 0.000000000000000000, 0.000000000000000000, 0.000000000000000000, 0.000000000000000000, 0.000000000000000000, 0.000000000000000000 ) ;
#10501 = UNCERTAINTY_MEASURE_WITH_UNIT (LENGTH_MEASURE( 1.000000000000000082E-05 ), #23442, 'distance_accuracy_value', 'NONE') ;
#10502 = ORIENTED_EDGE ( 'NONE', *, *, #23687, .T. ) ;
#10503 = CARTESIAN_POINT ( 'NONE',  ( 0.4296318976989615401, 0.1458850421962473720, -1.934055118110236338 ) ) ;
#10504 = EDGE_LOOP ( 'NONE', ( #12820, #14209, #26077 ) ) ;
#10505 = CARTESIAN_POINT ( 'NONE',  ( -0.5072939182192724994, -0.5338842954723621581, 0.1206349394395838659 ) ) ;
#10506 = CARTESIAN_POINT ( 'NONE',  ( 0.3726024258163779246, 4.695363739110452099E-17, -3.115157480314960647 ) ) ;
#10507 = CARTESIAN_POINT ( 'NONE',  ( 0.5043504886477717664, -0.1712563538833085097, 1.747047244094488194 ) ) ;
#10508 = EDGE_CURVE ( 'NONE', #18891, #10943, #22660, .T. ) ;
#10509 = DIRECTION ( 'NONE',  ( 0.6234898018587331503, -0.7818314824680301367, 0.000000000000000000 ) ) ;
#10510 = AXIS2_PLACEMENT_3D ( 'NONE', #25965, #4493, #17210 ) ;
#10511 = VERTEX_POINT ( 'NONE', #6204 ) ;
#10512 = EDGE_CURVE ( 'NONE', #13350, #2437, #19316, .T. ) ;
#10513 = B_SPLINE_CURVE_WITH_KNOTS ( 'NONE', 3,
 ( #1987, #16973, #12721, #14880, #19079, #25588 ),
 .UNSPECIFIED., .F., .F.,
 ( 4, 2, 4 ),
 ( 0.000000000000000000, 0.2500000000000000000, 0.5000000000000000000 ),
 .UNSPECIFIED. ) ;
#10514 = DIRECTION ( 'NONE',  ( 0.000000000000000000, 0.000000000000000000, 1.000000000000000000 ) ) ;
#10515 = CARTESIAN_POINT ( 'NONE',  ( -0.6034159556099095711, -0.5269038574519832041, 0.9872771499260571959 ) ) ;
#10516 = DIRECTION ( 'NONE',  ( 1.000000000000000000, 0.000000000000000000, 0.000000000000000000 ) ) ;
#10517 = CARTESIAN_POINT ( 'NONE',  ( 0.2227458012931471387, 0.3858827008519146728, -1.934055118110236560 ) ) ;
#10518 = ADVANCED_FACE ( 'NONE', ( #4213 ), #10553, .F. ) ;
#10519 = ORIENTED_EDGE ( 'NONE', *, *, #23397, .F. ) ;
#10520 = CARTESIAN_POINT ( 'NONE',  ( -0.1775730735577452091, -0.3074993854542726335, 1.953740157480315043 ) ) ;
#10521 = VERTEX_POINT ( 'NONE', #17065 ) ;
#10522 = CIRCLE ( 'NONE', #3747, 0.4980314960629921295 ) ;
#10523 = CARTESIAN_POINT ( 'NONE',  ( -0.5218358954157312768, -0.3040829563514129141, -0.2949399236599603569 ) ) ;
#10525 = CARTESIAN_POINT ( 'NONE',  ( 0.5417097841048533757, -0.1839420097223136985, 0.9399606299212598381 ) ) ;
#10524 = CARTESIAN_POINT ( 'NONE',  ( -0.2118615749922468650, -0.5840192333899535404, 0.2574803149606298969 ) ) ;
#10526 = ADVANCED_FACE ( 'NONE', ( #25822 ), #19046, .T. ) ;
#10527 = TOROIDAL_SURFACE ( 'NONE', #212, 0.3198827364362346048, 0.01377952755905511792 ) ;
#10528 = VERTEX_POINT ( 'NONE', #14696 ) ;
#10529 = CARTESIAN_POINT ( 'NONE',  ( 0.3334645669291338987, -1.243457723967850148, -0.6813714283177954023 ) ) ;
#10530 = DIRECTION ( 'NONE',  ( -1.000000000000000000, 1.224646799147346305E-16, 0.000000000000000000 ) ) ;
#10531 = DIRECTION ( 'NONE',  ( 0.000000000000000000, -0.000000000000000000, 1.000000000000000000 ) ) ;
#10532 = B_SPLINE_CURVE_WITH_KNOTS ( 'NONE', 3,
 ( #5995, #3863, #14479, #12335, #23086, #21096, #3714, #4146, #20954, #1599, #10203, #16871, #25480, #6143, #14774, #23379, #25326, #14902 ),
 .UNSPECIFIED., .F., .F.,
 ( 4, 2, 2, 2, 2, 2, 2, 2, 4 ),
 ( 0.000000000000000000, 0.2275410946275231994, 0.3413116419412837166, 0.4550821892550442893, 0.5688527365688048620, 0.6826232838825654348, 0.7395085575394457766, 0.7963938311963262295, 0.9101643785100869133 ),
 .UNSPECIFIED. ) ;
#10533 = CARTESIAN_POINT ( 'NONE',  ( 0.09660931395005890876, 0.3606853515406323596, -3.115157480314960647 ) ) ;
#10534 = CARTESIAN_POINT ( 'NONE',  ( -0.01288382813972184689, 0.2165354330708661457, -3.646653543307086576 ) ) ;
#10535 = CARTESIAN_POINT ( 'NONE',  ( -0.09842519685039370636, 0.07874015748031495954, 0.04546065111729331171 ) ) ;
#10536 = DIRECTION ( 'NONE',  ( 0.000000000000000000, -0.000000000000000000, -1.000000000000000000 ) ) ;
#10537 = CIRCLE ( 'NONE', #20460, 0.2847264097284254447 ) ;
#10538 = CARTESIAN_POINT ( 'NONE',  ( 0.6791338582677166613, 0.000000000000000000, -0.7480314960629921295 ) ) ;
#10539 = ORIENTED_EDGE ( 'NONE', *, *, #11383, .F. ) ;
#10540 = CARTESIAN_POINT ( 'NONE',  ( 0.4954734376820387198, 0.2860009521624328754, 0.9399606299212598381 ) ) ;
#10541 = CIRCLE ( 'NONE', #2837, 0.3180687940323247975 ) ;
#10542 = ORIENTED_EDGE ( 'NONE', *, *, #20406, .F. ) ;
#10543 = DIRECTION ( 'NONE',  ( 0.000000000000000000, 0.000000000000000000, 1.000000000000000000 ) ) ;
#10544 = CARTESIAN_POINT ( 'NONE',  ( -0.3013593406941685315, 0.3597456680659448791, 0.07637630773773090853 ) ) ;
#10545 = CARTESIAN_POINT ( 'NONE',  ( -0.4954415918530846175, -0.1327036767659680039, 1.766732283464566899 ) ) ;
#10546 = ORIENTED_EDGE ( 'NONE', *, *, #20884, .T. ) ;
#10547 = EDGE_CURVE ( 'NONE', #11118, #19022, #23303, .T. ) ;
#10548 = ORIENTED_EDGE ( 'NONE', *, *, #21821, .F. ) ;
#10549 = CARTESIAN_POINT ( 'NONE',  ( -0.3460635936744816399, -0.09269288654274071559, -3.115157480314960647 ) ) ;
#10550 = ORIENTED_EDGE ( 'NONE', *, *, #1608, .T. ) ;
#10551 = CARTESIAN_POINT ( 'NONE',  ( 0.4930758245789425009, 0.08754571829529310401, 0.2574803149606298969 ) ) ;
#10552 = ( NAMED_UNIT ( * ) PLANE_ANGLE_UNIT ( ) SI_UNIT ( $, .RADIAN. ) ) ;
#10553 = CYLINDRICAL_SURFACE ( 'NONE', #1908, 0.3346456692913385988 ) ;
#10554 = EDGE_CURVE ( 'NONE', #22901, #15797, #26259, .T. ) ;
#10555 = AXIS2_PLACEMENT_3D ( 'NONE', #5974, #11899, #18952 ) ;
#10556 = CARTESIAN_POINT ( 'NONE',  ( 0.04380447413659065842, -0.3324885138898235892, 1.973425196850393970 ) ) ;
#10557 = EDGE_LOOP ( 'NONE', ( #13332, #22184, #11915, #27760 ) ) ;
#10558 = ORIENTED_EDGE ( 'NONE', *, *, #5552, .T. ) ;
#10559 = DIRECTION ( 'NONE',  ( 1.000000000000000000, 0.000000000000000000, 0.000000000000000000 ) ) ;
#10560 = DIRECTION ( 'NONE',  ( 0.000000000000000000, 0.000000000000000000, 1.000000000000000000 ) ) ;
#10561 = ORIENTED_EDGE ( 'NONE', *, *, #1343, .F. ) ;
#10562 = ORIENTED_EDGE ( 'NONE', *, *, #15166, .T. ) ;
#10563 = VERTEX_POINT ( 'NONE', #1807 ) ;
#10564 = CARTESIAN_POINT ( 'NONE',  ( -0.1669771619559717590, -0.4570419016572346282, 0.09284957166232934989 ) ) ;
#10565 = AXIS2_PLACEMENT_3D ( 'NONE', #3126, #11753, #1309 ) ;
#10566 = CARTESIAN_POINT ( 'NONE',  ( -0.3412792617076849111, 0.05967164814832635888, 0.1377952755905512139 ) ) ;
#10567 = AXIS2_PLACEMENT_3D ( 'NONE', #7032, #13511, #15527 ) ;
#10568 = CARTESIAN_POINT ( 'NONE',  ( -0.02573449447784514899, 0.3139714872872414464, -3.643448523124805050 ) ) ;
#10569 = CARTESIAN_POINT ( 'NONE',  ( 0.1570092758121686138, -0.4330450457732857861, 0.1903859678454303539 ) ) ;
#10570 = VERTEX_POINT ( 'NONE', #19870 ) ;
#10571 = EDGE_CURVE ( 'NONE', #15240, #10641, #26266, .T. ) ;
#10572 = CARTESIAN_POINT ( 'NONE',  ( -0.6707652279343464530, -0.1538768215239710857, 0.1322834645669291320 ) ) ;
#10573 = AXIS2_PLACEMENT_3D ( 'NONE', #5944, #27407, #16254 ) ;
#10574 = DIRECTION ( 'NONE',  ( -1.000000000000000000, 0.000000000000000000, 0.000000000000000000 ) ) ;
#10575 = DIRECTION ( 'NONE',  ( 0.000000000000000000, 0.000000000000000000, 1.000000000000000000 ) ) ;
#10576 = CARTESIAN_POINT ( 'NONE',  ( -0.5833027994817057138, -0.2586580032347411962, 0.2101318059641304747 ) ) ;
#10577 = CARTESIAN_POINT ( 'NONE',  ( -0.09842519685039370636, 0.2165354330708661457, -3.548228346456693050 ) ) ;
#10578 = DIRECTION ( 'NONE',  ( 0.000000000000000000, 1.000000000000000000, 0.000000000000000000 ) ) ;
#10579 = CYLINDRICAL_SURFACE ( 'NONE', #20062, 0.4010740433761567081 ) ;
#10581 = EDGE_CURVE ( 'NONE', #13772, #2049, #6883, .T. ) ;
#10580 = AXIS2_PLACEMENT_3D ( 'NONE', #12013, #11585, #9592 ) ;
#10582 = CARTESIAN_POINT ( 'NONE',  ( 0.02576258753921353492, 0.2165354330708661457, -3.176774343053047733 ) ) ;
#10583 = ORIENTED_EDGE ( 'NONE', *, *, #16080, .F. ) ;
#10584 = AXIS2_PLACEMENT_3D ( 'NONE', #12930, #17716, #4724 ) ;
#10585 = EDGE_CURVE ( 'NONE', #6542, #11692, #4359, .T. ) ;
#10586 = ORIENTED_EDGE ( 'NONE', *, *, #7177, .F. ) ;
#10587 = CARTESIAN_POINT ( 'NONE',  ( 0.03008364706454716778, 0.1136516277932334562, 0.1968503937007874127 ) ) ;
#10588 = FACE_OUTER_BOUND ( 'NONE', #6777, .T. ) ;
#10589 = DIRECTION ( 'NONE',  ( -1.000000000000000000, 0.000000000000000000, 0.000000000000000000 ) ) ;
#10590 = CARTESIAN_POINT ( 'NONE',  ( 0.3362148458988273303, 0.4382482975805419012, 0.9202755905511811330 ) ) ;
#10591 = ORIENTED_EDGE ( 'NONE', *, *, #17152, .F. ) ;
#10592 = EDGE_CURVE ( 'NONE', #1086, #247, #10925, .T. ) ;
#10593 = AXIS2_PLACEMENT_3D ( 'NONE', #17982, #15631, #13086 ) ;
#10594 = CARTESIAN_POINT ( 'NONE',  ( 0.3759206409296169116, 0.2989751379763687655, 0.2362204724409450174 ) ) ;
#10595 = ORIENTED_EDGE ( 'NONE', *, *, #22601, .T. ) ;
#10596 = CARTESIAN_POINT ( 'NONE',  ( 0.000000000000000000, 0.4724409448818898127, 0.000000000000000000 ) ) ;
#10597 = CARTESIAN_POINT ( 'NONE',  ( 0.2243804351485034487, 0.2666304421164708005, 0.1589462317787528611 ) ) ;
#10598 = DIRECTION ( 'NONE',  ( -0.000000000000000000, -1.000000000000000000, -0.000000000000000000 ) ) ;
#10599 = CARTESIAN_POINT ( 'NONE',  ( 0.000000000000000000, 0.000000000000000000, 0.2362204724409449064 ) ) ;
#10600 = DIRECTION ( 'NONE',  ( 0.000000000000000000, 0.4702444477782121712, -0.8825362085114493160 ) ) ;
#10601 = EDGE_CURVE ( 'NONE', #23254, #12366, #12739, .T. ) ;
#10602 = AXIS2_PLACEMENT_3D ( 'NONE', #12111, #9711, #18593 ) ;
#10603 = ORIENTED_EDGE ( 'NONE', *, *, #18237, .F. ) ;
#10604 = DIRECTION ( 'NONE',  ( -0.9790454724845842893, -0.1018208755700880375, -0.1763589297585410332 ) ) ;
#10605 = CARTESIAN_POINT ( 'NONE',  ( 6.557635703933409897E-17, 0.3771653543307084688, 0.07637549214372833795 ) ) ;
#10606 = CARTESIAN_POINT ( 'NONE',  ( -0.3268939675028499914, -0.1881330340946393564, 0.07637795275590551769 ) ) ;
#10607 = AXIS2_PLACEMENT_3D ( 'NONE', #853, #20056, #9440 ) ;
#10608 = ORIENTED_EDGE ( 'NONE', *, *, #21762, .F. ) ;
#10609 = CARTESIAN_POINT ( 'NONE',  ( 0.07874015748031495954, 0.04546065111729338803, -0.4724409448818898127 ) ) ;
#10610 = DIRECTION ( 'NONE',  ( 1.000000000000000000, 0.000000000000000000, 0.000000000000000000 ) ) ;
#10611 = CARTESIAN_POINT ( 'NONE',  ( -0.4954156765914823346, 0.2860899518036844058, 0.9399606299212598381 ) ) ;
#10612 = CARTESIAN_POINT ( 'NONE',  ( 0.1603262695921948977, -0.4410554214326551370, 0.07637549214372854611 ) ) ;
#10613 = ORIENTED_EDGE ( 'NONE', *, *, #15491, .F. ) ;
#10614 = CARTESIAN_POINT ( 'NONE',  ( -0.1791101711253741402, 0.3102827802123027667, -3.115157480314961980 ) ) ;
#10615 = CIRCLE ( 'NONE', #24596, 0.4692913385826771866 ) ;
#10616 = EDGE_CURVE ( 'NONE', #25542, #12210, #11742, .T. ) ;
#10617 = ORIENTED_EDGE ( 'NONE', *, *, #11897, .F. ) ;
#10618 = CIRCLE ( 'NONE', #19198, 0.3937007874015748254 ) ;
#10619 = EDGE_CURVE ( 'NONE', #9720, #661, #11660, .T. ) ;
#10620 = CARTESIAN_POINT ( 'NONE',  ( 0.3382184156748877513, 0.3855916753034390188, -1.550196850393700920 ) ) ;
#10621 = CARTESIAN_POINT ( 'NONE',  ( -0.1838445375782518376, -0.5417516942599310825, 0.9399606299212600602 ) ) ;
#10622 = CARTESIAN_POINT ( 'NONE',  ( -1.928513779527558736E-17, 0.000000000000000000, -0.4448818897637791814 ) ) ;
#10623 = FACE_BOUND ( 'NONE', #25852, .T. ) ;
#10624 = CARTESIAN_POINT ( 'NONE',  ( 0.3511586785139784728, -0.4004922687719658647, 1.747047244094488416 ) ) ;
#10625 = CARTESIAN_POINT ( 'NONE',  ( -0.3015429802558983741, -0.1746717017761129087, 0.1589462317904963562 ) ) ;
#10626 = VERTEX_POINT ( 'NONE', #5157 ) ;
#10627 = CONICAL_SURFACE ( 'NONE', #24165, 0.08876456692913387014, 0.7853981624999977207 ) ;
#10628 = CARTESIAN_POINT ( 'NONE',  ( -0.6205631318075456315, -0.4724394499398413827, -0.9954595798869798617 ) ) ;
#10629 = CARTESIAN_POINT ( 'NONE',  ( -0.07874186976011487982, 0.3051029058891214230, -3.212186138815604330 ) ) ;
#10630 = CARTESIAN_POINT ( 'NONE',  ( 0.3020979083622633565, 0.3591256245826334181, 0.07637795275590551769 ) ) ;
#10631 = CARTESIAN_POINT ( 'NONE',  ( 0.4222761783103636257, 0.5043089796496124100, 0.1461456498321524189 ) ) ;
#10632 = CARTESIAN_POINT ( 'NONE',  ( -0.3267210193396165585, -0.1884333032645074957, 0.1992150590373740204 ) ) ;
#10633 = CARTESIAN_POINT ( 'NONE',  ( 0.000000000000000000, 0.000000000000000000, 0.07637795275590551769 ) ) ;
#10634 = VERTEX_POINT ( 'NONE', #15385 ) ;
#10635 = AXIS2_PLACEMENT_3D ( 'NONE', #20979, #6295, #27485 ) ;
#10636 = FACE_OUTER_BOUND ( 'NONE', #8996, .T. ) ;
#10637 = SPHERICAL_SURFACE ( 'NONE', #26762, 0.1299232283464566984 ) ;
#10638 = CARTESIAN_POINT ( 'NONE',  ( -0.2169784220115218709, -0.4520537072531055078, 0.1643955689481572668 ) ) ;
#10639 = DIRECTION ( 'NONE',  ( 1.000000000000000000, 0.000000000000000000, 0.000000000000000000 ) ) ;
#10640 = CARTESIAN_POINT ( 'NONE',  ( -0.06441834428466709783, -0.4889536969035322977, -1.569881889763779625 ) ) ;
#10641 = VERTEX_POINT ( 'NONE', #7284 ) ;
#10642 = EDGE_CURVE ( 'NONE', #24215, #3934, #3695, .T. ) ;
#10643 = DIRECTION ( 'NONE',  ( -1.000000000000000000, 1.224646799147353454E-16, 0.000000000000000000 ) ) ;
#10644 = CARTESIAN_POINT ( 'NONE',  ( -0.2006393256663304703, -0.4069519308876202168, -1.934055118110236338 ) ) ;
#10645 = CIRCLE ( 'NONE', #3895, 0.03937007874015744507 ) ;
#10646 = CARTESIAN_POINT ( 'NONE',  ( 0.1715719712213541193, -0.4696414150092599882, 0.1259302777268271334 ) ) ;
#10647 = LINE ( 'NONE', #11827, #14878 ) ;
#10648 = ORIENTED_EDGE ( 'NONE', *, *, #8421, .F. ) ;
#10650 = ORIENTED_EDGE ( 'NONE', *, *, #1033, .T. ) ;
#10649 = ADVANCED_FACE ( 'NONE', ( #21992 ), #26225, .F. ) ;
#10651 = CARTESIAN_POINT ( 'NONE',  ( -0.5439522672647024715, -0.2528481198474323288, -0.2762448575629318781 ) ) ;
#10652 = LENGTH_MEASURE_WITH_UNIT ( LENGTH_MEASURE( 0.02539999999999999897 ), #25775 ) ;
#10653 = CARTESIAN_POINT ( 'NONE',  ( 0.5314960629921260393, -0.03478633594540021801, 1.747047244094488194 ) ) ;
#10654 = CARTESIAN_POINT ( 'NONE',  ( -0.4620608682196457040, 0.08206165078054665496, 0.07637795275590551769 ) ) ;
#10655 = CARTESIAN_POINT ( 'NONE',  ( -0.6708219662590886312, -0.1536294932067314989, 0.3401591245381555551 ) ) ;
#10656 = CARTESIAN_POINT ( 'NONE',  ( -0.6205616028481958368, -0.4724399524669597450, 0.9954595399567032210 ) ) ;
#10657 = CYLINDRICAL_SURFACE ( 'NONE', #22699, 0.1771653543307086798 ) ;
#10658 = FACE_BOUND ( 'NONE', #16051, .T. ) ;
#10659 = CARTESIAN_POINT ( 'NONE',  ( -0.3019498226894488102, 0.3592501948414881796, 0.1992142434433716580 ) ) ;
#10660 = ORIENTED_EDGE ( 'NONE', *, *, #21353, .F. ) ;
#10661 = PRODUCT_DEFINITION_FORMATION_WITH_SPECIFIED_SOURCE ( 'ANY', '', #25836, .NOT_KNOWN. ) ;
#10662 = CARTESIAN_POINT ( 'NONE',  ( -0.5634947805916841190, -0.2083173938535096414, -0.2632452328862202595 ) ) ;
#10663 = DIRECTION ( 'NONE',  ( 1.000000000000000000, 0.000000000000000000, 0.000000000000000000 ) ) ;
#10664 = ORIENTED_EDGE ( 'NONE', *, *, #5649, .F. ) ;
#10665 = CARTESIAN_POINT ( 'NONE',  ( -0.3482225189666507403, -0.4539000224941303063, 0.9399606299212598381 ) ) ;
#10666 = AXIS2_PLACEMENT_3D ( 'NONE', #24477, #13612, #5128 ) ;
#10667 = CARTESIAN_POINT ( 'NONE',  ( 0.3102399269716953345, -0.8727316232512619676, -0.5905643219437008984 ) ) ;
#10668 = DIRECTION ( 'NONE',  ( -1.000000000000000000, 0.000000000000000000, 0.000000000000000000 ) ) ;
#10669 = PLANE ( 'NONE',  #2739 ) ;
#10670 = ADVANCED_BREP_SHAPE_REPRESENTATION ( 'Deep Groove Ball Bearing 15x28x7', ( #21329, #11588 ), #2565 ) ;
#10671 = CIRCLE ( 'NONE', #18333, 0.01181102362204724046 ) ;
#10672 = CARTESIAN_POINT ( 'NONE',  ( -0.1651192144506243575, -0.3349073414798197645, -3.115157480314960647 ) ) ;
#10673 = DIRECTION ( 'NONE',  ( 0.000000000000000000, 1.000000000000000000, 0.000000000000000000 ) ) ;
#10674 = B_SPLINE_CURVE_WITH_KNOTS ( 'NONE', 3,
 ( #717, #7347, #24705, #24570, #20626, #17910, #18484, #15825, #26687, #5222, #999, #9589, #1142, #18197, #7486, #16385, #18339, #14134, #6087, #3509, #10024, #16517, #1831, #12139, #8061, #19055, #16813, #25568, #18773, #16672, #17086, #27554, #1404, #25281, #18625, #5657, #14725, #12700, #10292, #14577, #10576, #23176, #23328, #25139, #14282, #27829, #5801, #21041, #27262, #3954, #18913, #22892, #14851, #7916, #14426, #16952, #19200, #3655, #23467, #5942, #20905, #21333, #1688, #23032, #1967, #12430, #21189, #3811, #27688, #4094, #12283, #8339, #1549, #23732, #4236, #171, #8875, #8744, #13387, #42, #22015, #17364, #26113, #21743, #11276, #12975, #11002, #1108, #7595, #3049, #5333 ),
 .UNSPECIFIED., .F., .F.,
 ( 4, 2, 1, 1, 2, 2, 1, 1, 1, 1, 1, 1, 2, 2, 2, 2, 1, 1, 1, 2, 2, 2, 1, 1, 1, 2, 2, 2, 1, 1, 1, 1, 2, 2, 2, 1, 1, 1, 2, 2, 2, 2, 2, 1, 1, 1, 1, 2, 2, 2, 2, 2, 1, 1, 1, 1, 2, 2, 2, 4 ),
 ( 0.000000000000000000, 0.03125000000001444678, 0.04687500000002166323, 0.05468750000002530615, 0.05859375000002713801, 0.06250000000002896294, 0.07812500000003637368, 0.08593750000004005130, 0.08984375000004191092, 0.09179687500004279910, 0.09277343750004320155, 0.09326171875004343748, 0.09350585937504350686, 0.09375000000004357625, 0.1015625000000450612, 0.1054687500000458245, 0.1074218750000461992, 0.1083984375000463934, 0.1088867187500464906, 0.1091308593750465322, 0.1093750000000465739, 0.1171875000000476841, 0.1210937500000482531, 0.1230468750000485167, 0.1240234375000486139, 0.1245117187500486694, 0.1250000000000487110, 0.1562500000000492661, 0.1718750000000495992, 0.1796875000000497935, 0.1835937500000499600, 0.1855468750000500711, 0.1865234375000500988, 0.1875000000000500988, 0.2187500000000488221, 0.2343750000000482114, 0.2421875000000479061, 0.2460937500000477673, 0.2480468750000476841, 0.2500000000000476286, 0.3750000000000428546, 0.4375000000000404676, 0.4687500000000393019, 0.4843750000000386913, 0.4921875000000383582, 0.4960937500000381917, 0.4980468750000381362, 0.4990234375000380251, 0.5000000000000378586, 0.6250000000000266454, 0.6875000000000210942, 0.7187500000000183187, 0.7343750000000169864, 0.7421875000000162093, 0.7460937500000158762, 0.7480468750000156541, 0.7490234375000155431, 0.7500000000000154321, 0.8750000000000076605, 1.000000000000000000 ),
 .UNSPECIFIED. ) ;
#10675 = DIRECTION ( 'NONE',  ( 0.000000000000000000, -1.000000000000000000, 0.000000000000000000 ) ) ;
#10676 = FACE_BOUND ( 'NONE', #3487, .T. ) ;
#10677 = EDGE_CURVE ( 'NONE', #11062, #24440, #19952, .T. ) ;
#10678 = CARTESIAN_POINT ( 'NONE',  ( 0.000000000000000000, 0.000000000000000000, -3.149606299191693548 ) ) ;
#10679 = EDGE_CURVE ( 'NONE', #14218, #22411, #6042, .T. ) ;
#10680 = CARTESIAN_POINT ( 'NONE',  ( -0.6118978891064095205, 0.1074467966294590654, 0.2574819594177531479 ) ) ;
#10681 = B_SPLINE_CURVE_WITH_KNOTS ( 'NONE', 3,
 ( #8745, #17366, #11003, #6638, #23874, #17090 ),
 .UNSPECIFIED., .F., .F.,
 ( 4, 2, 4 ),
 ( 0.3864984308775630262, 0.3881911340211369743, 0.3898838371647110335 ),
 .UNSPECIFIED. ) ;
#10682 = ADVANCED_FACE ( 'NONE', ( #15774 ), #13243, .T. ) ;
#10683 = VERTEX_POINT ( 'NONE', #9243 ) ;
#10684 = LINE ( 'NONE', #19301, #8754 ) ;
#10685 = ORIENTED_EDGE ( 'NONE', *, *, #22328, .F. ) ;
#10686 = EDGE_CURVE ( 'NONE', #15627, #3542, #20140, .T. ) ;
#10687 = ORIENTED_EDGE ( 'NONE', *, *, #5424, .F. ) ;
#10688 = DIRECTION ( 'NONE',  ( 0.000000000000000000, 0.000000000000000000, -1.000000000000000000 ) ) ;
#10689 = CARTESIAN_POINT ( 'NONE',  ( 0.3242071728275346953, -0.4225965726692721969, 1.747047244094488194 ) ) ;
#10690 = CARTESIAN_POINT ( 'NONE',  ( -0.2564944395515788567, -0.4441657790107717552, 1.766732283464566899 ) ) ;
#10691 = CARTESIAN_POINT ( 'NONE',  ( 0.7874015748031496509, 0.3931603432736094361, 0.1747896609116821598 ) ) ;
#10692 = ORIENTED_EDGE ( 'NONE', *, *, #27699, .F. ) ;
#10693 = CIRCLE ( 'NONE', #14311, 0.3722026523000413478 ) ;
#10694 = COLOUR_RGB ( '', 0.08235294, 0.09019608, 0.10196078) ;
#10695 = VERTEX_POINT ( 'NONE', #15902 ) ;
#10697 = CARTESIAN_POINT ( 'NONE',  ( 0.1791601451668921319, 0.3102476824511487541, -3.115157480314960647 ) ) ;
#10696 = CARTESIAN_POINT ( 'NONE',  ( 0.6055690743987126590, -0.2581485381169807414, -0.4471263839182408883 ) ) ;
#10698 = ORIENTED_EDGE ( 'NONE', *, *, #21675, .F. ) ;
#10699 = CARTESIAN_POINT ( 'NONE',  ( -0.1599629598573824862, -0.4411872753631803090, 0.07637795275590551769 ) ) ;
#10700 = ( NAMED_UNIT ( * ) SI_UNIT ( $, .STERADIAN. ) SOLID_ANGLE_UNIT ( ) ) ;
#10701 = DIRECTION ( 'NONE',  ( 0.000000000000000000, 0.000000000000000000, 1.000000000000000000 ) ) ;
#10702 = CARTESIAN_POINT ( 'NONE',  ( 0.04380447413659061678, 0.3324885138898235892, 1.973425196850393970 ) ) ;
#10703 = VERTEX_POINT ( 'NONE', #13783 ) ;
#10704 = ORIENTED_EDGE ( 'NONE', *, *, #2195, .T. ) ;
#10705 = CARTESIAN_POINT ( 'NONE',  ( -0.4763861460130593972, 0.1275996891957734969, -1.550196850393700920 ) ) ;
#10706 = VERTEX_POINT ( 'NONE', #22403 ) ;
#10707 = ORIENTED_EDGE ( 'NONE', *, *, #7921, .F. ) ;
#10708 = ORIENTED_EDGE ( 'NONE', *, *, #2574, .F. ) ;
#10709 = CARTESIAN_POINT ( 'NONE',  ( 0.07874015748031495954, 0.04546065111729338803, -0.3779527559055118058 ) ) ;
#10710 = ADVANCED_FACE ( 'NONE', ( #940 ), #11885, .F. ) ;
#10711 = AXIS2_PLACEMENT_3D ( 'NONE', #23221, #8100, #8239 ) ;
#10712 = CARTESIAN_POINT ( 'NONE',  ( -0.1968503937007874127, -0.07874015748031495954, 0.04546065111729338803 ) ) ;
#10713 = DIRECTION ( 'NONE',  ( 1.000000000000000000, 0.000000000000000000, 0.000000000000000000 ) ) ;
#10714 = AXIS2_PLACEMENT_3D ( 'NONE', #5136, #22240, #781 ) ;
#10715 = DIRECTION ( 'NONE',  ( 0.000000000000000000, 0.000000000000000000, -1.000000000000000000 ) ) ;
#10716 = ORIENTED_EDGE ( 'NONE', *, *, #6939, .F. ) ;
#10717 = B_SPLINE_SURFACE_WITH_KNOTS ( 'NONE', 2, 3, ( 
 ( #823, #11412, #26655, #26252, #24676, #13525, #15933, #24535, #22571, #22149, #2777, #5187, #6912, #683, #13816, #22019, #22431, #4771, #15535, #3053, #11689, #20310, #26803, #5336, #24134, #14396, #10265, #14546, #21011, #5773, #18744, #27379, #1520, #8033, #3338, #24826, #18310, #11978, #23006, #9994, #18453, #20453, #1380, #24964, #20596, #23145, #1248, #5626, #27525, #11832, #6057, #20739, #27101, #7747, #16637, #7603, #25251, #1113, #5912, #3627, #3778, #16360, #14254, #14688, #12251, #26956 ),
 ( #20872, #18879, #10130, #12112, #8168, #12397, #16778, #14099, #25391, #3198, #9712, #1659, #16223, #18594, #5487, #22713, #22862, #3484, #27236, #21713, #14825, #19309, #4067, #25673, #8576, #23571, #17467, #9, #26081, #6743, #17194, #10832, #4203, #12809, #2340, #23294, #6601, #25811, #21437, #3920, #6460, #12944, #21574, #19447, #8975, #18119, #6873, #2883, #22470, #18592, #7175, #7601, #16078, #11977, #15931, #13666, #12110, #22430, #13815, #1112, #5483, #22711, #27098, #15796, #20595, #3482 ),
 ( #20736, #24674, #1379, #24963, #26654, #14097, #24399, #1246, #9710, #9992, #5047, #3196, #22283, #22570, #18309, #3337, #9850, #18451, #9413, #13962, #7746, #18016, #5185, #16359, #26954, #966, #5623, #20309, #22861, #14252, #2919, #11548, #20163, #7312, #822, #3052, #5335, #24823, #11688, #11829, #9556, #18162, #26802, #20451, #7449, #16222, #27523, #8032, #14541, #27235, #6054, #25388, #16775, #21153, #10128, #10689, #21434, #18742, #14686, #12250, #10408, #12538, #2075, #19165, #20869, #23002 ) ),
 .UNSPECIFIED., .F., .T., .F.,
 ( 3, 3 ),
 ( 4, 2, 2, 2, 2, 2, 2, 2, 2, 2, 2, 2, 2, 2, 2, 2, 2, 2, 2, 2, 2, 2, 2, 2, 2, 2, 2, 2, 2, 2, 2, 2, 4 ),
 ( 0.000000000000000000, 1.000000000000000000 ),
 ( 0.000000000000000000, 0.1963495408493620697, 0.3926990816987241395, 0.5890486225480862092, 0.7853981633974482790, 0.9817477042468103487, 1.178097245096172418, 1.374446785945534488, 1.570796326794896558, 1.767145867644258628, 1.963495408493620697, 2.159844949342982545, 2.356194490192344837, 2.552544031041707129, 2.748893571891068976, 2.945243112740430824, 3.141592653589793116, 3.337942194439155408, 3.534291735288517255, 3.730641276137879103, 3.926990816987241395, 4.123340357836603687, 4.319689898685965090, 4.516039439535327382, 4.712388980384689674, 4.908738521234051966, 5.105088062083414258, 5.301437602932775661, 5.497787143782137953, 5.694136684631500245, 5.890486225480861648, 6.086835766330223940, 6.283185307179586232 ),
 .UNSPECIFIED. ) ;
#10718 = EDGE_CURVE ( 'NONE', #15474, #11206, #1957, .T. ) ;
#10719 = MECHANICAL_DESIGN_GEOMETRIC_PRESENTATION_REPRESENTATION (  '', ( #22902 ), #12971 ) ;
#10720 = CARTESIAN_POINT ( 'NONE',  ( 0.1490609433615242285, -0.2393035190771456711, -0.4144858534716441278 ) ) ;
#10721 = CARTESIAN_POINT ( 'NONE',  ( -0.07874015748031495954, -0.03414999754207796723, -0.4724409448818898127 ) ) ;
#10722 = CONTEXT_DEPENDENT_SHAPE_REPRESENTATION ( #24601, #24467 ) ;
#10723 = ADVANCED_FACE ( 'NONE', ( #25213 ), #24070, .F. ) ;
#10724 = EDGE_CURVE ( 'NONE', #26289, #25001, #14359, .T. ) ;
#10725 = CARTESIAN_POINT ( 'NONE',  ( 0.1520645003680120011, -0.4909313315697558799, -0.05587710509957795335 ) ) ;
#10726 = CARTESIAN_POINT ( 'NONE',  ( 0.1512365701434773002, -0.2842731118987109618, 0.3980489349105370556 ) ) ;
#10727 = CARTESIAN_POINT ( 'NONE',  ( 0.1660519377394881757, -2.925196850393700920, 0.7678753104628740500 ) ) ;
#10728 = CARTESIAN_POINT ( 'NONE',  ( 0.1200170377978880126, 0.4465874321618644172, -1.928289503579157183 ) ) ;
#10729 = EDGE_CURVE ( 'NONE', #22996, #24094, #22545, .T. ) ;
#10730 = CARTESIAN_POINT ( 'NONE',  ( -0.6131838103401908713, 1.106933345738153607, 0.07395176699543236365 ) ) ;
#10731 = CARTESIAN_POINT ( 'NONE',  ( 0.000000000000000000, 0.8661417322803149910, 0.000000000000000000 ) ) ;
#10732 = CARTESIAN_POINT ( 'NONE',  ( 0.08600259748440877705, 0.2165354330708661457, -3.223068998490982384 ) ) ;
#10733 = EDGE_LOOP ( 'NONE', ( #2352, #19796 ) ) ;
#10734 = CARTESIAN_POINT ( 'NONE',  ( 0.3362336590883683307, 0.1141709026133588128, 1.953740157480315043 ) ) ;
#10735 = AXIS2_PLACEMENT_3D ( 'NONE', #21104, #2025, #4151 ) ;
#10736 = CARTESIAN_POINT ( 'NONE',  ( 0.3062557396315260250, -0.6341756901077876263, 0.3281099440165241576 ) ) ;
#10737 = EDGE_CURVE ( 'NONE', #16391, #24778, #21869, .T. ) ;
#10738 = ORIENTED_EDGE ( 'NONE', *, *, #24251, .F. ) ;
#10739 = EDGE_LOOP ( 'NONE', ( #10417, #5634, #20788, #11113 ) ) ;
#10740 = CARTESIAN_POINT ( 'NONE',  ( 0.000000000000000000, 0.000000000000000000, 0.1322834645669291320 ) ) ;
#10741 = DIRECTION ( 'NONE',  ( 0.000000000000000000, 1.000000000000000000, 0.000000000000000000 ) ) ;
#10742 = CARTESIAN_POINT ( 'NONE',  ( -0.07214854559198564943, -0.5476281405333169872, 0.9202755905511811330 ) ) ;
#10743 = DIRECTION ( 'NONE',  ( 0.000000000000000000, 0.000000000000000000, 1.000000000000000000 ) ) ;
#10744 = ORIENTED_EDGE ( 'NONE', *, *, #20443, .F. ) ;
#10745 = DIRECTION ( 'NONE',  ( 0.000000000000000000, 0.000000000000000000, 1.000000000000000000 ) ) ;
#10746 = DIRECTION ( 'NONE',  ( -0.000000000000000000, -0.000000000000000000, -1.000000000000000000 ) ) ;
#10747 = CARTESIAN_POINT ( 'NONE',  ( -0.2362204724409449064, -0.6299212598425196763, 7.714310545810098438E-17 ) ) ;
#10748 = CARTESIAN_POINT ( 'NONE',  ( 0.5383572925355968319, -0.3100567972183901899, 0.09685039370078740717 ) ) ;
#10749 = CARTESIAN_POINT ( 'NONE',  ( -0.4716287720745061529, -0.1069935333114224313, 0.2008762816207269042 ) ) ;
#10750 = AXIS2_PLACEMENT_3D ( 'NONE', #11431, #20333, #26824 ) ;
#10751 = ADVANCED_FACE ( 'NONE', ( #20422 ), #13172, .T. ) ;
#10752 = ORIENTED_EDGE ( 'NONE', *, *, #5465, .T. ) ;
#10753 = CARTESIAN_POINT ( 'NONE',  ( -0.1189624676717062624, -0.3253923344978156829, 0.1276989850592374631 ) ) ;
#10754 = DIRECTION ( 'NONE',  ( 0.000000000000000000, 0.000000000000000000, -1.000000000000000000 ) ) ;
#10755 = CARTESIAN_POINT ( 'NONE',  ( 0.000000000000000000, 0.000000000000000000, -0.07578740157480315376 ) ) ;
#10756 = ADVANCED_FACE ( 'NONE', ( #22830 ), #27165, .F. ) ;
#10757 = DIRECTION ( 'NONE',  ( -1.000000000000000000, 0.000000000000000000, 0.000000000000000000 ) ) ;
#10758 = CARTESIAN_POINT ( 'NONE',  ( 0.5131133041954354379, -0.2529800193559368360, 0.9399606299212598381 ) ) ;
#10759 = VECTOR ( 'NONE', #16829, 39.37007874015748143 ) ;
#10760 = CARTESIAN_POINT ( 'NONE',  ( 0.000000000000000000, 0.000000000000000000, 0.3543307086614173040 ) ) ;
#10761 = DIRECTION ( 'NONE',  ( 0.000000000000000000, -1.000000000000000000, 0.000000000000000000 ) ) ;
#10762 = VERTEX_POINT ( 'NONE', #3450 ) ;
#10763 = CARTESIAN_POINT ( 'NONE',  ( -0.1151354519025668821, 0.3392634445560395173, -3.115157480314961091 ) ) ;
#10764 = EDGE_LOOP ( 'NONE', ( #6510, #12950 ) ) ;
#10765 = CIRCLE ( 'NONE', #1728, 0.2362204724225640262 ) ;
#10766 = VERTEX_POINT ( 'NONE', #27208 ) ;
#10767 = B_SPLINE_CURVE_WITH_KNOTS ( 'NONE', 3,
 ( #16367, #24970, #3785, #25116 ),
 .UNSPECIFIED., .F., .F.,
 ( 4, 4 ),
 ( 0.000000000000000000, 0.0002837997277716974506 ),
 .UNSPECIFIED. ) ;
#10768 = AXIS2_PLACEMENT_3D ( 'NONE', #16076, #2916, #26652 ) ;
#10769 = CARTESIAN_POINT ( 'NONE',  ( -0.4210617728879400001, -0.2437762437905965363, 0.1075369453512742129 ) ) ;
#10770 = PLANE ( 'NONE',  #3065 ) ;
#10771 = CIRCLE ( 'NONE', #3546, 0.1771653543307086798 ) ;
#10772 = FACE_OUTER_BOUND ( 'NONE', #24118, .T. ) ;
#10773 = ORIENTED_EDGE ( 'NONE', *, *, #14373, .F. ) ;
#10774 = CARTESIAN_POINT ( 'NONE',  ( -0.3263749705684267921, -0.1890319631540330891, 0.1992125984251968684 ) ) ;
#10775 = ORIENTED_EDGE ( 'NONE', *, *, #18332, .T. ) ;
#10776 = ORIENTED_EDGE ( 'NONE', *, *, #13942, .T. ) ;
#10777 = CARTESIAN_POINT ( 'NONE',  ( -0.2992781133269515892, -0.6197069291944330427, 0.1322834645669291320 ) ) ;
#10778 = AXIS2_PLACEMENT_3D ( 'NONE', #6785, #19642, #17511 ) ;
#10779 = CARTESIAN_POINT ( 'NONE',  ( -0.2395669291338582696, 0.000000000000000000, -0.4566929133858267376 ) ) ;
#10780 = ORIENTED_EDGE ( 'NONE', *, *, #16085, .T. ) ;
#10781 = LINE ( 'NONE', #17559, #21139 ) ;
#10782 = DIRECTION ( 'NONE',  ( 0.000000000000000000, -1.000000000000000000, 0.000000000000000000 ) ) ;
#10783 = ORIENTED_EDGE ( 'NONE', *, *, #14264, .T. ) ;
#10784 = DIRECTION ( 'NONE',  ( 0.000000000000000000, 0.000000000000000000, -1.000000000000000000 ) ) ;
#10785 = CARTESIAN_POINT ( 'NONE',  ( 0.03532354024591712049, -0.8267716535433071723, 0.000000000000000000 ) ) ;
#10786 = ADVANCED_FACE ( 'NONE', ( #5305 ), #16193, .T. ) ;
#10787 = AXIS2_PLACEMENT_3D ( 'NONE', #25658, #1923, #27648 ) ;
#10788 = UNCERTAINTY_MEASURE_WITH_UNIT (LENGTH_MEASURE( 1.000000000000000082E-05 ), #24609, 'distance_accuracy_value', 'NONE') ;
#10789 = CARTESIAN_POINT ( 'NONE',  ( -0.3979194638820524044, 0.2297883689023302312, -1.928289503579153630 ) ) ;
#10790 = VECTOR ( 'NONE', #26899, 39.37007874015748143 ) ;
#10791 = AXIS2_PLACEMENT_3D ( 'NONE', #27519, #27231, #8165 ) ;
#10792 = CARTESIAN_POINT ( 'NONE',  ( 0.2315507648392299000, -0.4792806379917101678, 0.3401574803149606252 ) ) ;
#10793 = CARTESIAN_POINT ( 'NONE',  ( -0.5744851493158656952, 0.4591414886146410468, 0.1960773254330283877 ) ) ;
#10794 = EDGE_LOOP ( 'NONE', ( #3437, #5979, #6990 ) ) ;
#10795 = AXIS2_PLACEMENT_3D ( 'NONE', #19396, #19679, #21521 ) ;
#10796 = CARTESIAN_POINT ( 'NONE',  ( -0.5252801253069795395, -0.4102412259628235858, 0.001906318767970118216 ) ) ;
#10797 = PLANE ( 'NONE',  #11815 ) ;
#10798 = CARTESIAN_POINT ( 'NONE',  ( -0.2663596103035690277, -0.4612490782034817105, 1.747047244094488194 ) ) ;
#10799 = SURFACE_STYLE_FILL_AREA ( #23802 ) ;
#10800 = ORIENTED_EDGE ( 'NONE', *, *, #27340, .T. ) ;
#10801 = CARTESIAN_POINT ( 'NONE',  ( -0.1608692170993913650, -0.4408576787418653775, 0.07637630773773071424 ) ) ;
#10802 = CARTESIAN_POINT ( 'NONE',  ( 0.4173228346456693272, 0.000000000000000000, 0.4488188976377953110 ) ) ;
#10803 = CARTESIAN_POINT ( 'NONE',  ( -0.5118110236220472231, 0.000000000000000000, -0.01377952755905511792 ) ) ;
#10804 = CARTESIAN_POINT ( 'NONE',  ( -0.2712680014834641939, 0.3534612032198612974, -1.934055118110237004 ) ) ;
#10805 = VERTEX_POINT ( 'NONE', #5457 ) ;
#10806 = AXIS2_PLACEMENT_3D ( 'NONE', #3634, #24973, #5196 ) ;
#10807 = CARTESIAN_POINT ( 'NONE',  ( -0.7432982829791772161, 0.3208553412839740826, 0.1963361843227200976 ) ) ;
#10808 = ORIENTED_EDGE ( 'NONE', *, *, #578, .T. ) ;
#10809 = CARTESIAN_POINT ( 'NONE',  ( -0.4296318976990082805, 0.1458850421962457622, -1.934055118110236338 ) ) ;
#10810 = CYLINDRICAL_SURFACE ( 'NONE', #18894, 1.377952755905512472 ) ;
#10811 = CIRCLE ( 'NONE', #19382, 0.1082677165354330728 ) ;
#10812 = CARTESIAN_POINT ( 'NONE',  ( 0.3334645669291338987, -1.269546425348450747, -0.8304542831125020230 ) ) ;
#10813 = CARTESIAN_POINT ( 'NONE',  ( -0.5708661417322835607, 0.000000000000000000, 0.9399606299212598381 ) ) ;
#10814 = AXIS2_PLACEMENT_3D ( 'NONE', #8204, #6096, #18378 ) ;
#10815 = CARTESIAN_POINT ( 'NONE',  ( -0.5112608635011182123, 0.3373130994319499809, -0.2804599709653767814 ) ) ;
#10816 = DIRECTION ( 'NONE',  ( 1.000000000000000000, 0.000000000000000000, 0.000000000000000000 ) ) ;
#10817 = CARTESIAN_POINT ( 'NONE',  ( 0.2962590301041578278, 0.2272836761397798999, -3.115157480314960647 ) ) ;
#10818 = DIRECTION ( 'NONE',  ( 0.000000000000000000, 0.000000000000000000, 1.000000000000000000 ) ) ;
#10819 = ( NAMED_UNIT ( * ) SI_UNIT ( $, .STERADIAN. ) SOLID_ANGLE_UNIT ( ) ) ;
#10820 = DIRECTION ( 'NONE',  ( 0.000000000000000000, 1.000000000000000000, 0.000000000000000000 ) ) ;
#10821 = CARTESIAN_POINT ( 'NONE',  ( 0.1516263115863346334, 0.1971492568089275588, 0.4530651079966787620 ) ) ;
#10822 = EDGE_CURVE ( 'NONE', #13016, #2225, #5594, .T. ) ;
#10823 = CARTESIAN_POINT ( 'NONE',  ( 0.0005847768872538051076, 0.4787829797961309919, 0.08349695147752299318 ) ) ;
#10824 = CONICAL_SURFACE ( 'NONE', #18947, 0.3066721922917531873, 0.5845243560369969282 ) ;
#10825 = ORIENTED_EDGE ( 'NONE', *, *, #24578, .F. ) ;
#10826 = DIRECTION ( 'NONE',  ( -0.9790454724845839563, 0.2036417511401769909, 0.000000000000000000 ) ) ;
#10827 = AXIS2_PLACEMENT_3D ( 'NONE', #22307, #7335, #15953 ) ;
#10828 = ORIENTED_EDGE ( 'NONE', *, *, #27216, .F. ) ;
#10829 = DIRECTION ( 'NONE',  ( 0.000000000000000000, 0.000000000000000000, 1.000000000000000000 ) ) ;
#10830 = CARTESIAN_POINT ( 'NONE',  ( 0.000000000000000000, 0.000000000000000000, 0.4062992125984251635 ) ) ;
#10831 = CARTESIAN_POINT ( 'NONE',  ( -0.4771018889076559244, 0.3804760601893846794, 0.3661437007874016047 ) ) ;
#10832 = CARTESIAN_POINT ( 'NONE',  ( -0.5085118447801413311, 0.06699507805369032953, 1.747047244094488194 ) ) ;
#10833 = DIRECTION ( 'NONE',  ( -1.000000000000000000, 0.000000000000000000, 0.000000000000000000 ) ) ;
#10834 = VERTEX_POINT ( 'NONE', #18422 ) ;
#10835 = ORIENTED_EDGE ( 'NONE', *, *, #9584, .T. ) ;
#10837 = CARTESIAN_POINT ( 'NONE',  ( -0.2180698645301767380, -0.2842490391651532611, -3.115157480314960647 ) ) ;
#10836 = CARTESIAN_POINT ( 'NONE',  ( 0.5754648248638597474, 0.4579130143396930031, 0.1960773254437022384 ) ) ;
#10838 = ORIENTED_EDGE ( 'NONE', *, *, #10995, .F. ) ;
#10839 = CARTESIAN_POINT ( 'NONE',  ( -0.09139240964747699647, 0.07874015748031500117, -0.02109836160874975844 ) ) ;
#10840 = ORIENTED_EDGE ( 'NONE', *, *, #8552, .T. ) ;
#10841 = FACE_OUTER_BOUND ( 'NONE', #26254, .T. ) ;
#10842 = CARTESIAN_POINT ( 'NONE',  ( 0.3339160553493882300, 1.090203750159222551, -0.7502486126520099274 ) ) ;
#10843 = CARTESIAN_POINT ( 'NONE',  ( -0.08676778863011123943, 0.3239425792934299553, 1.953740157480315043 ) ) ;
#10844 = ORIENTED_EDGE ( 'NONE', *, *, #6615, .F. ) ;
#10845 = ADVANCED_FACE ( 'NONE', ( #18562 ), #20862, .T. ) ;
#10846 = LINE ( 'NONE', #17740, #179 ) ;
#10847 = ORIENTED_EDGE ( 'NONE', *, *, #440, .F. ) ;
#10848 = VERTEX_POINT ( 'NONE', #23541 ) ;
#10849 = ORIENTED_EDGE ( 'NONE', *, *, #3074, .F. ) ;
#10850 = CARTESIAN_POINT ( 'NONE',  ( 0.3722026523000413478, 4.558167867734008572E-17, -0.1309055118110236116 ) ) ;
#10851 = CIRCLE ( 'NONE', #24834, 0.5322834645669292097 ) ;
#10852 = EDGE_CURVE ( 'NONE', #13505, #19099, #14110, .T. ) ;
#10853 = CARTESIAN_POINT ( 'NONE',  ( -0.09139240964747710749, -0.07874015748031500117, -1.188614124534770567E-17 ) ) ;
#10854 = CARTESIAN_POINT ( 'NONE',  ( 0.000000000000000000, 0.000000000000000000, 0.09685039370078740717 ) ) ;
#10855 = CARTESIAN_POINT ( 'NONE',  ( 0.1579154690117922366, -0.4355388305902855306, 0.2048502515516587574 ) ) ;
#10856 = ORIENTED_EDGE ( 'NONE', *, *, #14054, .F. ) ;
#10857 = AXIS2_PLACEMENT_3D ( 'NONE', #15408, #16853, #18661 ) ;
#10858 = CARTESIAN_POINT ( 'NONE',  ( 0.4092416079569000109, -5.011764252623336046E-17, -0.05856299212598425896 ) ) ;
#10859 = CARTESIAN_POINT ( 'NONE',  ( 0.1522836969815822838, -0.2938892803218252081, 0.3971963147669425598 ) ) ;
#10860 = CARTESIAN_POINT ( 'NONE',  ( -0.4465874321618641951, 0.1200170377978884984, -1.928289503579156960 ) ) ;
#10861 = CARTESIAN_POINT ( 'NONE',  ( -0.6003936137737501122, 1.122047331090473721, 0.009609423979446465522 ) ) ;
#10862 = FACE_OUTER_BOUND ( 'NONE', #20491, .T. ) ;
#10863 = CARTESIAN_POINT ( 'NONE',  ( -0.5314974819112029403, 0.03488411621207041652, 1.747047244094488194 ) ) ;
#10864 = EDGE_CURVE ( 'NONE', #2522, #9569, #286, .T. ) ;
#10865 = CARTESIAN_POINT ( 'NONE',  ( -0.09586345222254787080, 0.1968503937007873850, -3.246875207736363844 ) ) ;
#10866 = ORIENTED_EDGE ( 'NONE', *, *, #13914, .T. ) ;
#10867 = CARTESIAN_POINT ( 'NONE',  ( -0.3056525133678795747, 0.3651631491437063448, 0.2330651857751106226 ) ) ;
#10868 = CARTESIAN_POINT ( 'NONE',  ( 0.3543307086614173596, 0.000000000000000000, 1.953740157480315043 ) ) ;
#10869 = VERTEX_POINT ( 'NONE', #6019 ) ;
#10870 = EDGE_CURVE ( 'NONE', #25476, #13715, #11056, .T. ) ;
#10871 = CARTESIAN_POINT ( 'NONE',  ( -0.1968503937007874127, -0.07874015748031495954, -0.04546065111729338803 ) ) ;
#10872 = DIRECTION ( 'NONE',  ( 0.000000000000000000, 0.000000000000000000, -1.000000000000000000 ) ) ;
#10873 = EDGE_CURVE ( 'NONE', #25509, #16023, #12291, .T. ) ;
#10874 = DIRECTION ( 'NONE',  ( 1.000000000000000000, 0.000000000000000000, 0.000000000000000000 ) ) ;
#10875 = EDGE_CURVE ( 'NONE', #4501, #26847, #23528, .T. ) ;
#10876 = EDGE_LOOP ( 'NONE', ( #3519, #6345 ) ) ;
#10877 = CARTESIAN_POINT ( 'NONE',  ( -0.3642352168757361786, -0.4152525734086467968, 0.9202755905511811330 ) ) ;
#10878 = DIMENSIONAL_EXPONENTS ( 1.000000000000000000, 0.000000000000000000, 0.000000000000000000, 0.000000000000000000, 0.000000000000000000, 0.000000000000000000, 0.000000000000000000 ) ;
#10879 = ADVANCED_FACE ( 'NONE', ( #26453 ), #26592, .T. ) ;
#10880 = FACE_OUTER_BOUND ( 'NONE', #12086, .T. ) ;
#10881 = ORIENTED_EDGE ( 'NONE', *, *, #17918, .T. ) ;
#10882 = FACE_OUTER_BOUND ( 'NONE', #12827, .T. ) ;
#10883 = LENGTH_MEASURE_WITH_UNIT ( LENGTH_MEASURE( 0.02539999999999999897 ), #19498 ) ;
#10885 = ADVANCED_FACE ( 'NONE', ( #8818 ), #18613, .F. ) ;
#10886 = DIRECTION ( 'NONE',  ( 0.000000000000000000, -1.000000000000000000, 0.000000000000000000 ) ) ;
#10887 = FACE_OUTER_BOUND ( 'NONE', #7619, .T. ) ;
#10888 = CARTESIAN_POINT ( 'NONE',  ( -0.2564173815256688971, -0.4442189740297868839, -1.550196850393701142 ) ) ;
#10889 = ( NAMED_UNIT ( * ) SI_UNIT ( $, .STERADIAN. ) SOLID_ANGLE_UNIT ( ) ) ;
#10890 = AXIS2_PLACEMENT_3D ( 'NONE', #22947, #16722, #13902 ) ;
#10891 = DIRECTION ( 'NONE',  ( 0.000000000000000000, 0.000000000000000000, 1.000000000000000000 ) ) ;
#10892 = CARTESIAN_POINT ( 'NONE',  ( 0.2236164729197613887, 0.2672714825449903908, 0.1589462317899844046 ) ) ;
#10893 = DIRECTION ( 'NONE',  ( 1.000000000000000000, 0.000000000000000000, 0.000000000000000000 ) ) ;
#10894 = CARTESIAN_POINT ( 'NONE',  ( -0.2428345617565149384, 0.2885915454824177218, 0.07637795275590551769 ) ) ;
#10895 = DIRECTION ( 'NONE',  ( -0.5000000010362839475, 0.8660254031861397417, 0.000000000000000000 ) ) ;
#10896 = CARTESIAN_POINT ( 'NONE',  ( -0.5118110236220472231, 6.402768735150616610E-17, 1.747047244094488194 ) ) ;
#10897 = CIRCLE ( 'NONE', #21267, 0.09143349766193348271 ) ;
#10898 = CARTESIAN_POINT ( 'NONE',  ( 0.2860899518037616773, -0.4954156765914850546, 0.9399606299212598381 ) ) ;
#10899 = CARTESIAN_POINT ( 'NONE',  ( 0.1327957795771031180, -0.4954247181591464044, -1.550196850393700476 ) ) ;
#10900 = VERTEX_POINT ( 'NONE', #17957 ) ;
#10901 = DIRECTION ( 'NONE',  ( 1.000000000000000000, 0.000000000000000000, 0.000000000000000000 ) ) ;
#10902 = ORIENTED_EDGE ( 'NONE', *, *, #1628, .T. ) ;
#10903 = DIRECTION ( 'NONE',  ( 0.000000000000000000, 0.000000000000000000, 1.000000000000000000 ) ) ;
#10904 = VERTEX_POINT ( 'NONE', #24468 ) ;
#10905 = CARTESIAN_POINT ( 'NONE',  ( 0.000000000000000000, 0.000000000000000000, 0.2574803149606298969 ) ) ;
#10906 = ORIENTED_EDGE ( 'NONE', *, *, #27340, .F. ) ;
#10907 = EDGE_CURVE ( 'NONE', #15613, #4851, #2288, .T. ) ;
#10908 = AXIS2_PLACEMENT_3D ( 'NONE', #14298, #3678, #3531 ) ;
#10909 = CARTESIAN_POINT ( 'NONE',  ( -0.3771696032823899092, -0.4301590433674395419, 0.9399606299212597271 ) ) ;
#10910 = CARTESIAN_POINT ( 'NONE',  ( 0.4622285577935897893, 0.08111201067594568659, 0.07637630773773071424 ) ) ;
#10911 = CARTESIAN_POINT ( 'NONE',  ( -0.4527559054764771496, 5.544660704368294164E-17, -1.934055118110236338 ) ) ;
#10912 = DIRECTION ( 'NONE',  ( 0.000000000000000000, 0.000000000000000000, -1.000000000000000000 ) ) ;
#10913 = ORIENTED_EDGE ( 'NONE', *, *, #701, .T. ) ;
#10914 = EDGE_CURVE ( 'NONE', #21446, #4739, #9085, .T. ) ;
#10915 = FACE_OUTER_BOUND ( 'NONE', #20832, .T. ) ;
#10916 = ORIENTED_EDGE ( 'NONE', *, *, #26785, .F. ) ;
#10917 = CARTESIAN_POINT ( 'NONE',  ( -0.01202960507629146671, -0.3256422846268542948, -0.2993518939891427477 ) ) ;
#10918 = DIRECTION ( 'NONE',  ( -0.9790454724845840673, 0.1018208755700876073, -0.1763589297585415050 ) ) ;
#10919 = FACE_OUTER_BOUND ( 'NONE', #21859, .T. ) ;
#10920 = DIRECTION ( 'NONE',  ( -0.2384530002628483802, 0.000000000000000000, -0.9711540385879295911 ) ) ;
#10921 = CARTESIAN_POINT ( 'NONE',  ( 0.2981382804008161913, -0.6202561546315472629, 0.1322818203437344520 ) ) ;
#10922 = ORIENTED_EDGE ( 'NONE', *, *, #18912, .F. ) ;
#10923 = LINE ( 'NONE', #17681, #15296 ) ;
#10924 = DIRECTION ( 'NONE',  ( 1.000000000000000000, 0.000000000000000000, 0.000000000000000000 ) ) ;
#10925 = CIRCLE ( 'NONE', #14630, 2.066929133858267598 ) ;
#10926 = ADVANCED_FACE ( 'NONE', ( #26055 ), #19834, .F. ) ;
#10927 = CARTESIAN_POINT ( 'NONE',  ( 0.4555658499976260600, 0.06001958459474954211, -1.928289503579140529 ) ) ;
#10928 = TOROIDAL_SURFACE ( 'NONE', #24451, 0.4173228346456693272, 0.02362204724409448786 ) ;
#10929 = B_SPLINE_CURVE_WITH_KNOTS ( 'NONE', 3,
 ( #19963, #7381, #619, #9207, #13882, #24605 ),
 .UNSPECIFIED., .F., .F.,
 ( 4, 2, 4 ),
 ( 1.217380381967462011, 1.219305002860848086, 1.221229623754233939 ),
 .UNSPECIFIED. ) ;
#10930 = LINE ( 'NONE', #15972, #13068 ) ;
#10931 = CARTESIAN_POINT ( 'NONE',  ( -0.5604501195207933772, 0.4479362078532184155, 0.1601585119423933334 ) ) ;
#10932 = LINE ( 'NONE', #13326, #13023 ) ;
#10933 = CARTESIAN_POINT ( 'NONE',  ( -0.6165893942483189338, -0.1074060693884885814, -0.08465106059891655543 ) ) ;
#10934 = DIRECTION ( 'NONE',  ( 0.000000000000000000, 0.000000000000000000, 1.000000000000000000 ) ) ;
#10935 = EDGE_CURVE ( 'NONE', #25110, #19539, #17701, .T. ) ;
#10936 = CARTESIAN_POINT ( 'NONE',  ( 0.000000000000000000, 0.000000000000000000, -0.2204724409448818867 ) ) ;
#10937 = ADVANCED_FACE ( 'NONE', ( #2314 ), #11354, .F. ) ;
#10938 = CARTESIAN_POINT ( 'NONE',  ( 0.4325730547867440712, 5.297492069419787030E-17, -0.1740172276534823204 ) ) ;
#10939 = ADVANCED_FACE ( 'NONE', ( #9215 ), #13462, .T. ) ;
#10940 = CYLINDRICAL_SURFACE ( 'NONE', #4756, 0.09842519685039370636 ) ;
#10941 = DIRECTION ( 'NONE',  ( -0.9790454724845842893, 0.1018208755700880375, 0.1763589297585410332 ) ) ;
#10942 = ADVANCED_FACE ( 'NONE', ( #22087 ), #4578, .F. ) ;
#10943 = VERTEX_POINT ( 'NONE', #369 ) ;
#10944 = AXIS2_PLACEMENT_3D ( 'NONE', #9790, #14038, #10062 ) ;
#10945 = CARTESIAN_POINT ( 'NONE',  ( -0.6912180915490531152, 0.08120084520073209133, -0.2401638807511342344 ) ) ;
#10946 = VERTEX_POINT ( 'NONE', #13190 ) ;
#10947 = ORIENTED_EDGE ( 'NONE', *, *, #11730, .T. ) ;
#10948 = CARTESIAN_POINT ( 'NONE',  ( -0.6117062799105531523, 0.1085321106658068829, 0.2574803149606298969 ) ) ;
#10949 = CARTESIAN_POINT ( 'NONE',  ( 0.5189874374926378708, -0.1182276436463391700, 0.1322810039474935084 ) ) ;
#10950 = EDGE_LOOP ( 'NONE', ( #18419, #13501, #8781, #9084 ) ) ;
#10951 = CARTESIAN_POINT ( 'NONE',  ( 0.5708661417322835607, -0.03736310157557555522, 0.9399606299212598381 ) ) ;
#10952 = CARTESIAN_POINT ( 'NONE',  ( 0.1120675189988346587, -0.6505216398953739265, -0.1269869061606480332 ) ) ;
#10953 = DIRECTION ( 'NONE',  ( -0.7071067818211401734, 0.000000000000000000, -0.7071067805519547500 ) ) ;
#10954 = VECTOR ( 'NONE', #714, 39.37007874015748143 ) ;
#10955 = DIRECTION ( 'NONE',  ( 0.000000000000000000, -1.000000000000000000, 0.000000000000000000 ) ) ;
#10956 = CARTESIAN_POINT ( 'NONE',  ( -0.3726024258163779246, 0.000000000000000000, -3.115157480314960647 ) ) ;
#10957 = CARTESIAN_POINT ( 'NONE',  ( -0.6711032387266713251, -0.1523958994812759926, 0.3401574803149606252 ) ) ;
#10958 = CARTESIAN_POINT ( 'NONE',  ( 0.2982299571069384481, 0.3545282230944422630, 0.1494804571808522331 ) ) ;
#10959 = DIRECTION ( 'NONE',  ( -1.000000000000000000, 0.000000000000000000, 0.000000000000000000 ) ) ;
#10960 = EDGE_CURVE ( 'NONE', #23531, #23608, #27575, .T. ) ;
#10961 = ORIENTED_EDGE ( 'NONE', *, *, #20824, .T. ) ;
#10962 = LINE ( 'NONE', #12802, #1014 ) ;
#10963 = AXIS2_PLACEMENT_3D ( 'NONE', #27535, #4218, #21456 ) ;
#10964 = VECTOR ( 'NONE', #24592, 39.37007874015748143 ) ;
#10965 = ORIENTED_EDGE ( 'NONE', *, *, #10071, .T. ) ;
#10966 = CARTESIAN_POINT ( 'NONE',  ( 0.5021077788563528266, -0.1139291307083610677, 0.3251195115536875124 ) ) ;
#10967 = LINE ( 'NONE', #19593, #8182 ) ;
#10968 = AXIS2_PLACEMENT_3D ( 'NONE', #12953, #19604, #8985 ) ;
#10969 = CARTESIAN_POINT ( 'NONE',  ( 0.06699507805369657454, 0.5085118447801424413, 1.766732283464566899 ) ) ;
#10970 = ORIENTED_EDGE ( 'NONE', *, *, #608, .F. ) ;
#10971 = FACE_BOUND ( 'NONE', #19702, .T. ) ;
#10972 = ORIENTED_EDGE ( 'NONE', *, *, #6835, .T. ) ;
#10973 = CIRCLE ( 'NONE', #25415, 0.4173228346456693272 ) ;
#10974 = ORIENTED_EDGE ( 'NONE', *, *, #22805, .T. ) ;
#10975 = CARTESIAN_POINT ( 'NONE',  ( 0.2693339498142252042, 0.2362439534887496861, -3.115157480314960647 ) ) ;
#10976 = ORIENTED_EDGE ( 'NONE', *, *, #25033, .F. ) ;
#10977 = VECTOR ( 'NONE', #8738, 39.37007874015748143 ) ;
#10978 = CARTESIAN_POINT ( 'NONE',  ( -1.197070535079588716, 0.4724409448818898127, 1.078960298859116707 ) ) ;
#10979 = ORIENTED_EDGE ( 'NONE', *, *, #26249, .T. ) ;
#10980 = CARTESIAN_POINT ( 'NONE',  ( 0.000000000000000000, 0.5610236220472440971, 0.1771653543307086520 ) ) ;
#10981 = EDGE_CURVE ( 'NONE', #4492, #14265, #24926, .T. ) ;
#10982 = CARTESIAN_POINT ( 'NONE',  ( -0.2041304421298407168, -0.2660793235464189999, 1.953740157480315043 ) ) ;
#10983 = ORIENTED_EDGE ( 'NONE', *, *, #24079, .T. ) ;
#10984 = ORIENTED_EDGE ( 'NONE', *, *, #18252, .T. ) ;
#10985 = EDGE_CURVE ( 'NONE', #18210, #19765, #23611, .T. ) ;
#10986 = CARTESIAN_POINT ( 'NONE',  ( 0.3267210193396165585, -0.1884333032645078565, 0.1992150590373740204 ) ) ;
#10987 = CARTESIAN_POINT ( 'NONE',  ( 0.6118597084614606496, 0.1076640027107480246, 0.09684793308443542803 ) ) ;
#10988 = ORIENTED_EDGE ( 'NONE', *, *, #18348, .F. ) ;
#10989 = ORIENTED_EDGE ( 'NONE', *, *, #26425, .T. ) ;
#10990 = ORIENTED_EDGE ( 'NONE', *, *, #5390, .F. ) ;
#10991 = DIRECTION ( 'NONE',  ( -1.000000000000000000, 0.000000000000000000, 0.000000000000000000 ) ) ;
#10992 = CLOSED_SHELL ( 'NONE', ( #14896, #7530, #1466, #23241, #7309, #23008, #5261, #673, #6734, #19617, #737, #14132, #10479, #24149, #8018, #12943, #26471, #25138 ) ) ;
#10993 = VECTOR ( 'NONE', #21665, 39.37007874015748143 ) ;
#10994 = VECTOR ( 'NONE', #20601, 39.37007874015748143 ) ;
#10995 = EDGE_CURVE ( 'NONE', #12986, #19589, #2993, .T. ) ;
#10996 = CARTESIAN_POINT ( 'NONE',  ( 0.4245040230929275626, 1.106753849019775471, -0.3897420188601015689 ) ) ;
#10997 = DIRECTION ( 'NONE',  ( 0.000000000000000000, 0.000000000000000000, -1.000000000000000000 ) ) ;
#10998 = FACE_BOUND ( 'NONE', #7821, .T. ) ;
#10999 = VECTOR ( 'NONE', #2914, 39.37007874015748143 ) ;
#11000 = CARTESIAN_POINT ( 'NONE',  ( -0.0006345105826669216777, 0.4803145415259080786, 0.2529987172475652857 ) ) ;
#11001 = EDGE_CURVE ( 'NONE', #21048, #11355, #15476, .T. ) ;
#11002 = CARTESIAN_POINT ( 'NONE',  ( -0.3521695574743459733, -1.152827357733649638, -0.4707598252271103512 ) ) ;
#11003 = CARTESIAN_POINT ( 'NONE',  ( -0.5188885761056504231, -0.1186607836835326668, 0.1322810039474935084 ) ) ;
#11004 = DIRECTION ( 'NONE',  ( -1.000000000000000000, 0.000000000000000000, 0.000000000000000000 ) ) ;
#11005 = FILL_AREA_STYLE_COLOUR ( '', #9940 ) ;
#11006 = AXIS2_PLACEMENT_3D ( 'NONE', #20795, #1440, #8091 ) ;
#11007 = VERTEX_POINT ( 'NONE', #27036 ) ;
#11008 = CARTESIAN_POINT ( 'NONE',  ( 0.09842519684998451979, 0.1968503937008052596, -3.259751644589256703 ) ) ;
#11009 = ORIENTED_EDGE ( 'NONE', *, *, #13941, .F. ) ;
#11010 = VERTEX_POINT ( 'NONE', #7682 ) ;
#11011 = CARTESIAN_POINT ( 'NONE',  ( 0.000000000000000000, 0.03937007874015751446, 0.5511811023975373702 ) ) ;
#11012 = CARTESIAN_POINT ( 'NONE',  ( 0.3429876364231437824, -0.09193127540148529619, 1.953740157480314821 ) ) ;
#11013 = ORIENTED_EDGE ( 'NONE', *, *, #21838, .T. ) ;
#11014 = CARTESIAN_POINT ( 'NONE',  ( -0.3010840436257778974, 0.2313841235333766178, -3.100567304031763172 ) ) ;
#11015 = TOROIDAL_SURFACE ( 'NONE', #26791, 0.6102362204724409711, 0.1299212598425196763 ) ;
#11016 = CARTESIAN_POINT ( 'NONE',  ( -0.3149606299212598381, 0.6397637795275591399, 0.000000000000000000 ) ) ;
#11017 = CARTESIAN_POINT ( 'NONE',  ( 0.7168072604734050390, -0.1644124225522937965, 0.2763636194388741085 ) ) ;
#11018 = DIRECTION ( 'NONE',  ( 0.000000000000000000, -1.000000000000000000, 0.000000000000000000 ) ) ;
#11019 = AXIS2_PLACEMENT_3D ( 'NONE', #18733, #7874, #5762 ) ;
#11020 = VERTEX_POINT ( 'NONE', #1324 ) ;
#11021 = CARTESIAN_POINT ( 'NONE',  ( 0.1429116519061375268, 0.5335524835332416949, 0.9399606299212598381 ) ) ;
#11022 = DIRECTION ( 'NONE',  ( 0.000000000000000000, 0.000000000000000000, 1.000000000000000000 ) ) ;
#11023 = VERTEX_POINT ( 'NONE', #12051 ) ;
#11024 = DIRECTION ( 'NONE',  ( 0.000000000000000000, 0.000000000000000000, -1.000000000000000000 ) ) ;
#11025 = FACE_OUTER_BOUND ( 'NONE', #27422, .T. ) ;
#11026 = LINE ( 'NONE', #17520, #25341 ) ;
#11027 = CARTESIAN_POINT ( 'NONE',  ( -0.6562077975700453258, 2.612916929133858441E-14, 0.2362204724409449064 ) ) ;
#11028 = B_SPLINE_CURVE_WITH_KNOTS ( 'NONE', 3,
 ( #4253, #4389, #60, #12858, #8625, #17244 ),
 .UNSPECIFIED., .F., .F.,
 ( 4, 2, 4 ),
 ( 0.3000437156586439613, 0.3015484798814569989, 0.3030532441042709801 ),
 .UNSPECIFIED. ) ;
#11029 = CIRCLE ( 'NONE', #14668, 0.4842519685039370358 ) ;
#11030 = CARTESIAN_POINT ( 'NONE',  ( -0.1714649452450071054, -0.4705186852026070898, 0.09684793308443542803 ) ) ;
#11031 = CARTESIAN_POINT ( 'NONE',  ( -0.07874015748031495954, 0.1968503937007873850, -3.548228346456693050 ) ) ;
#11032 = CARTESIAN_POINT ( 'NONE',  ( -0.3149606299212598381, -0.6889763779527560139, 8.437527159479796553E-17 ) ) ;
#11033 = FACE_OUTER_BOUND ( 'NONE', #20009, .T. ) ;
#11034 = EDGE_CURVE ( 'NONE', #12707, #10268, #7802, .T. ) ;
#11035 = AXIS2_PLACEMENT_3D ( 'NONE', #7042, #23875, #17367 ) ;
#11036 = CARTESIAN_POINT ( 'NONE',  ( 0.2230788859036007821, 0.2650812153444456198, 0.1377952755905513527 ) ) ;
#11037 = ORIENTED_EDGE ( 'NONE', *, *, #27734, .T. ) ;
#11038 = CARTESIAN_POINT ( 'NONE',  ( -0.1480156394741914683, 0.5526079293737398146, 0.9399606299212598381 ) ) ;
#11039 = CIRCLE ( 'NONE', #25920, 0.1771653543307086520 ) ;
#11040 = CARTESIAN_POINT ( 'NONE',  ( -0.09139240964747702423, 0.07874015748031500117, -1.981023540891279271E-18 ) ) ;
#11041 = DIRECTION ( 'NONE',  ( 0.000000000000000000, 0.000000000000000000, 1.000000000000000000 ) ) ;
#11042 = EDGE_CURVE ( 'NONE', #27722, #18177, #19522, .T. ) ;
#11043 = EDGE_LOOP ( 'NONE', ( #27447, #2457, #23506, #20359 ) ) ;
#11044 = ADVANCED_FACE ( 'NONE', ( #26733 ), #26716, .F. ) ;
#11045 = ORIENTED_EDGE ( 'NONE', *, *, #1502, .F. ) ;
#11046 = AXIS2_PLACEMENT_3D ( 'NONE', #13486, #2613, #9106 ) ;
#11047 = ORIENTED_EDGE ( 'NONE', *, *, #22758, .F. ) ;
#11048 = CARTESIAN_POINT ( 'NONE',  ( 0.000000000000000000, 0.000000000000000000, -1.092739370078740131E-17 ) ) ;
#11049 = CARTESIAN_POINT ( 'NONE',  ( -0.7874015748031496509, 3.035194737559056185E-06, -1.475314960619023674 ) ) ;
#11050 = DIRECTION ( 'NONE',  ( -1.000000000000000000, 0.000000000000000000, 0.000000000000000000 ) ) ;
#11051 = CARTESIAN_POINT ( 'NONE',  ( 0.3411065095061436847, 0.06065137456822567580, 0.1276989850527261161 ) ) ;
#11052 = VERTEX_POINT ( 'NONE', #22648 ) ;
#11053 = CARTESIAN_POINT ( 'NONE',  ( -0.3100894960432669101, -0.1796141127297333773, 0.1805249803397054320 ) ) ;
#11054 = VERTEX_POINT ( 'NONE', #907 ) ;
#11055 = AXIS2_PLACEMENT_3D ( 'NONE', #15407, #21882, #1412 ) ;
#11056 = B_SPLINE_CURVE_WITH_KNOTS ( 'NONE', 3,
 ( #6571, #19421, #23403, #27629, #15196, #10232, #23677, #18846, #27488, #12509 ),
 .UNSPECIFIED., .F., .F.,
 ( 4, 2, 2, 2, 4 ),
 ( 0.000000000000000000, 0.2500000000000002776, 0.5000000000000005551, 0.7500000000000002220, 1.000000000000000000 ),
 .UNSPECIFIED. ) ;
#11057 = DIRECTION ( 'NONE',  ( 0.000000000000000000, 1.000000000000000000, 0.000000000000000000 ) ) ;
#11058 = CIRCLE ( 'NONE', #14212, 0.3771653543307086909 ) ;
#11059 = CARTESIAN_POINT ( 'NONE',  ( -0.6118978891064172920, 0.1074467966294249954, 0.09684874924366436433 ) ) ;
#11060 = DIRECTION ( 'NONE',  ( 0.000000000000000000, -1.000000000000000000, 0.000000000000000000 ) ) ;
#11061 = FACE_OUTER_BOUND ( 'NONE', #6030, .T. ) ;
#11062 = VERTEX_POINT ( 'NONE', #18530 ) ;
#11063 = DIRECTION ( 'NONE',  ( -0.000000000000000000, 1.000000000000000000, -0.000000000000000000 ) ) ;
#11064 = DIRECTION ( 'NONE',  ( -0.9790454724845839563, -0.1018208755700890228, -0.1763589297585420324 ) ) ;
#11065 = CARTESIAN_POINT ( 'NONE',  ( -0.3252100150720461658, 0.3707612262532960501, -1.550196850393700920 ) ) ;
#11066 = DIMENSIONAL_EXPONENTS ( 1.000000000000000000, 0.000000000000000000, 0.000000000000000000, 0.000000000000000000, 0.000000000000000000, 0.000000000000000000, 0.000000000000000000 ) ;
#11067 = AXIS2_PLACEMENT_3D ( 'NONE', #27241, #11836, #7607 ) ;
#11068 = CARTESIAN_POINT ( 'NONE',  ( 0.3030032861724964444, -0.3454440660767522098, -1.928289503579156516 ) ) ;
#11069 = ADVANCED_FACE ( 'NONE', ( #1453 ), #24611, .T. ) ;
#11070 = DIRECTION ( 'NONE',  ( 0.000000000000000000, 1.000000000000000000, 0.000000000000000000 ) ) ;
#11071 = EDGE_CURVE ( 'NONE', #26673, #16499, #5289, .T. ) ;
#11072 = TOROIDAL_SURFACE ( 'NONE', #18264, 0.7480314960629921295, 0.03937007874015747977 ) ;
#11073 = ADVANCED_FACE ( 'NONE', ( #16161 ), #5541, .T. ) ;
#11074 = CIRCLE ( 'NONE', #8367, 0.6299212598425196763 ) ;
#11075 = CARTESIAN_POINT ( 'NONE',  ( -0.6544535166833030937, -0.004037084301382362454, -0.2362204724409449064 ) ) ;
#11076 = DIRECTION ( 'NONE',  ( 1.000000000000000000, 0.000000000000000000, 0.000000000000000000 ) ) ;
#11077 = B_SPLINE_CURVE_WITH_KNOTS ( 'NONE', 3,
 ( #2192, #6577, #10949, #9221, #19574, #19707 ),
 .UNSPECIFIED., .F., .F.,
 ( 4, 2, 4 ),
 ( 0.3864984308775630262, 0.3881911340211369743, 0.3898838371647110335 ),
 .UNSPECIFIED. ) ;
#11078 = ORIENTED_EDGE ( 'NONE', *, *, #5935, .F. ) ;
#11079 = CARTESIAN_POINT ( 'NONE',  ( 0.3268939675028499914, -0.1881330340946397728, 0.1992125984251968684 ) ) ;
#11080 = CARTESIAN_POINT ( 'NONE',  ( -0.1141732283464566844, 0.5570866141732283561, 0.000000000000000000 ) ) ;
#11081 = CARTESIAN_POINT ( 'NONE',  ( -0.4055118110236220486, -0.4724409448818898127, 0.9954570744419881656 ) ) ;
#11082 = CARTESIAN_POINT ( 'NONE',  ( -0.08530183727034104657, 0.03937007874015747977, 0.06819097667594015144 ) ) ;
#11083 = AXIS2_PLACEMENT_3D ( 'NONE', #623, #9212, #22083 ) ;
#11084 = ORIENTED_EDGE ( 'NONE', *, *, #4876, .F. ) ;
#11085 = CARTESIAN_POINT ( 'NONE',  ( -0.7246715730664488042, 0.2211122077665220453, 0.05732876522465197439 ) ) ;
#11086 = EDGE_CURVE ( 'NONE', #14891, #16095, #21779, .T. ) ;
#11087 = ORIENTED_EDGE ( 'NONE', *, *, #26541, .T. ) ;
#11088 = ORIENTED_EDGE ( 'NONE', *, *, #6634, .T. ) ;
#11089 = DIRECTION ( 'NONE',  ( 0.000000000000000000, 0.000000000000000000, -1.000000000000000000 ) ) ;
#11090 = CARTESIAN_POINT ( 'NONE',  ( 8.810208661417323492E-17, -4.420669291338583154E-18, 0.000000000000000000 ) ) ;
#11091 = CARTESIAN_POINT ( 'NONE',  ( 0.000000000000000000, 0.07874015748662489822, -0.2952755905511805778 ) ) ;
#11092 = CARTESIAN_POINT ( 'NONE',  ( 0.3534635626042424428, -0.2712695779737102075, -1.934055118110236338 ) ) ;
#11093 = CARTESIAN_POINT ( 'NONE',  ( -0.2807137536170428715, 0.2462256503456040635, -3.115157480314960647 ) ) ;
#11094 = CARTESIAN_POINT ( 'NONE',  ( 1.857656692913385893E-16, 0.000000000000000000, 0.000000000000000000 ) ) ;
#11095 = FACE_OUTER_BOUND ( 'NONE', #5389, .T. ) ;
#11096 = FACE_OUTER_BOUND ( 'NONE', #7467, .T. ) ;
#11097 = ORIENTED_EDGE ( 'NONE', *, *, #3109, .T. ) ;
#11098 = CARTESIAN_POINT ( 'NONE',  ( 0.06441914069860960046, -0.4921259842519685179, -1.569881889763779625 ) ) ;
#11099 = ADVANCED_FACE ( 'NONE', ( #24757 ), #18668, .T. ) ;
#11100 = CIRCLE ( 'NONE', #18291, 0.1082677165354330312 ) ;
#11101 = EDGE_CURVE ( 'NONE', #6630, #20898, #13890, .T. ) ;
#11102 = EDGE_LOOP ( 'NONE', ( #4986, #22313, #12064, #24382, #24667, #12211 ) ) ;
#11103 = VERTEX_POINT ( 'NONE', #1190 ) ;
#11104 = CARTESIAN_POINT ( 'NONE',  ( 0.000000000000000000, 0.000000000000000000, 0.1322834645669291320 ) ) ;
#11105 = FACE_OUTER_BOUND ( 'NONE', #27290, .T. ) ;
#11106 = DIRECTION ( 'NONE',  ( 0.000000000000000000, 0.000000000000000000, -1.000000000000000000 ) ) ;
#11107 = ADVANCED_FACE ( 'NONE', ( #18089 ), #26287, .T. ) ;
#11108 = ORIENTED_EDGE ( 'NONE', *, *, #17282, .T. ) ;
#11109 = ORIENTED_EDGE ( 'NONE', *, *, #114, .F. ) ;
#11111 = CARTESIAN_POINT ( 'NONE',  ( -0.2962590301041579388, -0.2272836761397900585, -3.115157480314960647 ) ) ;
#11110 = FACE_BOUND ( 'NONE', #26859, .T. ) ;
#11112 = AXIS2_PLACEMENT_3D ( 'NONE', #10308, #6366, #6102 ) ;
#11113 = ORIENTED_EDGE ( 'NONE', *, *, #11181, .F. ) ;
#11114 = CARTESIAN_POINT ( 'NONE',  ( 0.3334645669291338987, -0.8041772776331653771, -0.9118913923173522784 ) ) ;
#11115 = DIRECTION ( 'NONE',  ( 0.000000000000000000, 1.000000000000000000, 0.000000000000000000 ) ) ;
#11116 = CARTESIAN_POINT ( 'NONE',  ( 0.02190250779246040100, 0.3346456692913385988, 1.953740157480315043 ) ) ;
#11117 = ORIENTED_EDGE ( 'NONE', *, *, #27640, .F. ) ;
#11118 = VERTEX_POINT ( 'NONE', #3275 ) ;
#11119 = CARTESIAN_POINT ( 'NONE',  ( -0.0006615832605804723319, 0.6212594902576319411, 0.2574803149606298969 ) ) ;
#11120 = CARTESIAN_POINT ( 'NONE',  ( 0.3937007874015748254, 0.000000000000000000, 0.02362204724409448786 ) ) ;
#11121 = ORIENTED_EDGE ( 'NONE', *, *, #6972, .F. ) ;
#11122 = ORIENTED_EDGE ( 'NONE', *, *, #14281, .F. ) ;
#11123 = ORIENTED_EDGE ( 'NONE', *, *, #746, .F. ) ;
#11124 = CARTESIAN_POINT ( 'NONE',  ( -0.4330708661417322913, 0.000000000000000000, 0.000000000000000000 ) ) ;
#11125 = DIRECTION ( 'NONE',  ( 0.000000000000000000, 1.000000000000000000, 0.000000000000000000 ) ) ;
#11126 = CARTESIAN_POINT ( 'NONE',  ( -0.06046497745473627949, 0.3092442853777944700, -3.626959870088829252 ) ) ;
#11127 = CARTESIAN_POINT ( 'NONE',  ( 0.7640955261426980449, 0.5878663239606607416, 0.09435744292894028551 ) ) ;
#11128 = VERTEX_POINT ( 'NONE', #14321 ) ;
#11129 = B_SPLINE_CURVE_WITH_KNOTS ( 'NONE', 3,
 ( #13477, #22107, #13077, #10958, #19582, #261 ),
 .UNSPECIFIED., .F., .F.,
 ( 4, 2, 4 ),
 ( 0.000000000000000000, 0.2500000000000000000, 0.5000000000000000000 ),
 .UNSPECIFIED. ) ;
#11130 = EDGE_CURVE ( 'NONE', #15627, #12477, #1464, .T. ) ;
#11131 = ORIENTED_EDGE ( 'NONE', *, *, #11690, .F. ) ;
#11132 = DIRECTION ( 'NONE',  ( 0.000000000000000000, 0.000000000000000000, 1.000000000000000000 ) ) ;
#11133 = AXIS2_PLACEMENT_3D ( 'NONE', #27672, #14703, #25827 ) ;
#11134 = EDGE_CURVE ( 'NONE', #21723, #19812, #586, .T. ) ;
#11135 = CARTESIAN_POINT ( 'NONE',  ( 0.1504231045792248644, -0.2747315525089227273, 0.3999795527262415273 ) ) ;
#11136 = EDGE_CURVE ( 'NONE', #7703, #2225, #17266, .T. ) ;
#11137 = CARTESIAN_POINT ( 'NONE',  ( 0.5869493968219645641, 0.2133897621573074832, 0.3696019098714952711 ) ) ;
#11138 = CARTESIAN_POINT ( 'NONE',  ( 0.07874015748031495954, 0.03414999754207796723, -0.4724409448818898127 ) ) ;
#11139 = CARTESIAN_POINT ( 'NONE',  ( 0.0006443779181942713890, 0.4960456921234573935, 0.1734435147384566500 ) ) ;
#11140 = ORIENTED_EDGE ( 'NONE', *, *, #1415, .F. ) ;
#11141 = CARTESIAN_POINT ( 'NONE',  ( -0.2952755905264887182, 3.616083068046089993E-17, -3.110236220451535694 ) ) ;
#11142 = VERTEX_POINT ( 'NONE', #12185 ) ;
#11143 = CYLINDRICAL_SURFACE ( 'NONE', #23914, 0.1082677165354330312 ) ;
#11144 = ( LENGTH_UNIT ( ) NAMED_UNIT ( * ) SI_UNIT ( $, .METRE. ) ) ;
#11145 = EDGE_LOOP ( 'NONE', ( #5308, #25346, #20750, #22071 ) ) ;
#11146 = DIRECTION ( 'NONE',  ( -0.000000000000000000, -1.000000000000000000, -0.000000000000000000 ) ) ;
#11147 = DIRECTION ( 'NONE',  ( -0.9009688679024190350, 0.4338837391175582314, 0.000000000000000000 ) ) ;
#11148 = CARTESIAN_POINT ( 'NONE',  ( 0.5981657849660177995, 0.000000000000000000, 0.000000000000000000 ) ) ;
#11149 = AXIS2_PLACEMENT_3D ( 'NONE', #15376, #6872, #17599 ) ;
#11150 = CARTESIAN_POINT ( 'NONE',  ( -0.4169216294785028087, -0.5582982840830001958, -0.4568332836680285003 ) ) ;
#11151 = ORIENTED_EDGE ( 'NONE', *, *, #2073, .T. ) ;
#11152 = CARTESIAN_POINT ( 'NONE',  ( -0.4382482975805320757, -0.3362148458988418187, 0.9202755905511811330 ) ) ;
#11153 = CARTESIAN_POINT ( 'NONE',  ( 0.07874015748031495954, -0.04546065111729338803, -0.4724409448818898127 ) ) ;
#11154 = ORIENTED_EDGE ( 'NONE', *, *, #6186, .T. ) ;
#11155 = B_SPLINE_CURVE_WITH_KNOTS ( 'NONE', 3,
 ( #3865, #5569, #12480, #14196 ),
 .UNSPECIFIED., .F., .F.,
 ( 4, 4 ),
 ( 0.000000000000000000, 1.000000000000000000 ),
 .UNSPECIFIED. ) ;
#11156 = DIRECTION ( 'NONE',  ( 0.000000000000000000, -1.000000000000000000, 0.000000000000000000 ) ) ;
#11157 = AXIS2_PLACEMENT_3D ( 'NONE', #11798, #7562, #13631 ) ;
#11158 = CARTESIAN_POINT ( 'NONE',  ( 0.1599629598573263645, -0.4411872753632007926, 0.1992125984251968684 ) ) ;
#11159 = CARTESIAN_POINT ( 'NONE',  ( 0.2956505864974370845, 0.3532288989643546095, 0.1903859677965938912 ) ) ;
#11160 = CARTESIAN_POINT ( 'NONE',  ( -0.5708661417322835607, 0.000000000000000000, 0.000000000000000000 ) ) ;
#11161 = CARTESIAN_POINT ( 'NONE',  ( 0.3204319178470658724, -0.6672004808835035883, 0.2562996996018049312 ) ) ;
#11162 = CARTESIAN_POINT ( 'NONE',  ( -0.06048688226688715697, 0.2165354330708661457, -3.626935712454874228 ) ) ;
#11163 = CARTESIAN_POINT ( 'NONE',  ( 0.01935208613492874971, 0.07974837009520491238, -0.4684893292439904489 ) ) ;
#11164 = PLANE ( 'NONE',  #4657 ) ;
#11165 = DIRECTION ( 'NONE',  ( -0.2036417511401761582, 0.4895227362422917006, -0.8478782506317886769 ) ) ;
#11166 = EDGE_CURVE ( 'NONE', #13935, #1342, #11847, .T. ) ;
#11167 = AXIS2_PLACEMENT_3D ( 'NONE', #23487, #10598, #21060 ) ;
#11168 = CARTESIAN_POINT ( 'NONE',  ( -5.645730259564185549E-17, 0.4692913385826772976, 0.07637549214372836570 ) ) ;
#11169 = CARTESIAN_POINT ( 'NONE',  ( 0.3123213164505638240, 0.3731274149336368251, 0.1827409795199129161 ) ) ;
#11170 = CARTESIAN_POINT ( 'NONE',  ( -0.4539000224940974992, -0.3482225189666513510, 0.9399606299212598381 ) ) ;
#11171 = ( GEOMETRIC_REPRESENTATION_CONTEXT ( 3 ) GLOBAL_UNCERTAINTY_ASSIGNED_CONTEXT ( ( #10788 ) ) GLOBAL_UNIT_ASSIGNED_CONTEXT ( ( #24609, #8852, #19605 ) ) REPRESENTATION_CONTEXT ( 'NONE', 'WORKASPACE' ) ) ;
#11172 = DIRECTION ( 'NONE',  ( 0.000000000000000000, 0.000000000000000000, -1.000000000000000000 ) ) ;
#11173 = PRODUCT_DEFINITION_SHAPE ( 'NONE', 'NONE',  #27889 ) ;
#11174 = CARTESIAN_POINT ( 'NONE',  ( -0.2847264097284254447, 3.551487965556214605E-17, -3.149606299191693548 ) ) ;
#11175 = CARTESIAN_POINT ( 'NONE',  ( -0.6299212598425196763, -0.4724409448818898127, 0.8182917201112794858 ) ) ;
#11176 = ORIENTED_EDGE ( 'NONE', *, *, #4865, .T. ) ;
#11177 = ORIENTED_EDGE ( 'NONE', *, *, #23690, .F. ) ;
#11178 = DIRECTION ( 'NONE',  ( 1.000000000000000000, 0.000000000000000000, 0.000000000000000000 ) ) ;
#11179 = DIRECTION ( 'NONE',  ( 0.000000000000000000, -1.000000000000000000, 0.000000000000000000 ) ) ;
#11180 = DIRECTION ( 'NONE',  ( -1.000000000000000000, 0.000000000000000000, 0.000000000000000000 ) ) ;
#11181 = EDGE_CURVE ( 'NONE', #1421, #26488, #5063, .T. ) ;
#11182 = CARTESIAN_POINT ( 'NONE',  ( 0.000000000000000000, 0.000000000000000000, 0.2362204724409449064 ) ) ;
#11183 = CIRCLE ( 'NONE', #20612, 0.09842519685039370636 ) ;
#11184 = ADVANCED_FACE ( 'NONE', ( #10772 ), #23512, .T. ) ;
#11185 = DIRECTION ( 'NONE',  ( -1.000000000000000000, 0.000000000000000000, -0.000000000000000000 ) ) ;
#11186 = AXIS2_PLACEMENT_3D ( 'NONE', #15990, #25870, #23759 ) ;
#11187 = CIRCLE ( 'NONE', #10280, 0.1771653543307086520 ) ;
#11188 = CARTESIAN_POINT ( 'NONE',  ( 0.1516263115863346334, 0.2937912646890004087, -0.3972688187320929099 ) ) ;
#11189 = CARTESIAN_POINT ( 'NONE',  ( 0.3126261861395013275, 3.828566581853849315E-17, -0.1464516454673935042 ) ) ;
#11190 = CARTESIAN_POINT ( 'NONE',  ( -2.073220866141732523E-16, 0.4724409448818898127, 1.692913385826771533 ) ) ;
#11191 = CARTESIAN_POINT ( 'NONE',  ( 0.000000000000000000, 0.000000000000000000, 0.2574803149606298969 ) ) ;
#11192 = DIRECTION ( 'NONE',  ( 0.000000000000000000, 0.000000000000000000, -1.000000000000000000 ) ) ;
#11193 = EDGE_CURVE ( 'NONE', #3390, #764, #6901, .T. ) ;
#11194 = ORIENTED_EDGE ( 'NONE', *, *, #129, .T. ) ;
#11195 = AXIS2_PLACEMENT_3D ( 'NONE', #21204, #23047, #10452 ) ;
#11196 = CARTESIAN_POINT ( 'NONE',  ( 7.955503286468943460E-18, 0.6102362204724409711, 0.3661437007874016047 ) ) ;
#11197 = DIRECTION ( 'NONE',  ( 1.000000000000000000, 0.000000000000000000, 0.000000000000000000 ) ) ;
#11198 = CARTESIAN_POINT ( 'NONE',  ( -0.3937007874015748254, 4.893765752498281459E-17, 0.3425196850393700809 ) ) ;
#11199 = PLANE ( 'NONE',  #1274 ) ;
#11200 = CARTESIAN_POINT ( 'NONE',  ( 0.3132247436403744478, 0.3723693495128845288, 0.1827409795189120778 ) ) ;
#11201 = CARTESIAN_POINT ( 'NONE',  ( 0.1669771619565829646, -0.4570419016589117867, 0.09284957166463024547 ) ) ;
#11202 = AXIS2_PLACEMENT_3D ( 'NONE', #2404, #4403, #6665 ) ;
#11203 = DIRECTION ( 'NONE',  ( -0.000000000000000000, -0.000000000000000000, -1.000000000000000000 ) ) ;
#11204 = CARTESIAN_POINT ( 'NONE',  ( -0.4055118110236220486, -0.4724409448818898127, 0.8182917201112794858 ) ) ;
#11205 = CARTESIAN_POINT ( 'NONE',  ( -0.4790936880893625349, 0.08507591033004376080, 0.09284957166262186590 ) ) ;
#11206 = VERTEX_POINT ( 'NONE', #8385 ) ;
#11207 = DIRECTION ( 'NONE',  ( 0.000000000000000000, 0.000000000000000000, 1.000000000000000000 ) ) ;
#11208 = AXIS2_PLACEMENT_3D ( 'NONE', #8084, #5969, #18942 ) ;
#11210 = DIRECTION ( 'NONE',  ( -1.000000000000000000, 0.000000000000000000, 0.000000000000000000 ) ) ;
#11209 = VECTOR ( 'NONE', #21483, 39.37007874015748143 ) ;
#11211 = CARTESIAN_POINT ( 'NONE',  ( 0.000000000000000000, 0.000000000000000000, 0.3059055118110236560 ) ) ;
#11212 = DIRECTION ( 'NONE',  ( 0.000000000000000000, 0.000000000000000000, 1.000000000000000000 ) ) ;
#11213 = CARTESIAN_POINT ( 'NONE',  ( -0.7246715730664488042, 0.1595564285404119931, -0.2516711161248811335 ) ) ;
#11214 = VERTEX_POINT ( 'NONE', #8651 ) ;
#11215 = EDGE_CURVE ( 'NONE', #14592, #24185, #10493, .T. ) ;
#11216 = CARTESIAN_POINT ( 'NONE',  ( 0.000000000000000000, 0.000000000000000000, 0.06614173228346456601 ) ) ;
#11217 = FACE_OUTER_BOUND ( 'NONE', #6930, .T. ) ;
#11218 = EDGE_CURVE ( 'NONE', #2222, #13772, #16376, .T. ) ;
#11219 = DIRECTION ( 'NONE',  ( 1.000000000000000000, 0.000000000000000000, 0.000000000000000000 ) ) ;
#11220 = EDGE_CURVE ( 'NONE', #25275, #10141, #9323, .T. ) ;
#11221 = CIRCLE ( 'NONE', #6260, 0.6212598425196850238 ) ;
#11222 = PLANE ( 'NONE',  #22678 ) ;
#11223 = CARTESIAN_POINT ( 'NONE',  ( 0.09762295995069811272, -0.3644697409450263215, -3.100567304031765836 ) ) ;
#11224 = ADVANCED_FACE ( 'NONE', ( #12886 ), #14139, .F. ) ;
#11225 = VECTOR ( 'NONE', #4833, 39.37007874015748143 ) ;
#11226 = DIRECTION ( 'NONE',  ( -0.000000000000000000, -1.000000000000000000, -0.000000000000000000 ) ) ;
#11227 = CARTESIAN_POINT ( 'NONE',  ( 0.2362204724225640262, 0.000000000000000000, -4.291338582656260670 ) ) ;
#11228 = CARTESIAN_POINT ( 'NONE',  ( 0.6476458834277908361, 0.1148891961917465482, 0.2081850588316230821 ) ) ;
#11229 = ORIENTED_EDGE ( 'NONE', *, *, #17978, .T. ) ;
#11230 = DIRECTION ( 'NONE',  ( 0.000000000000000000, 0.000000000000000000, 1.000000000000000000 ) ) ;
#11231 = ( GEOMETRIC_REPRESENTATION_CONTEXT ( 3 ) GLOBAL_UNCERTAINTY_ASSIGNED_CONTEXT ( ( #22596 ) ) GLOBAL_UNIT_ASSIGNED_CONTEXT ( ( #15709, #20217, #26705 ) ) REPRESENTATION_CONTEXT ( 'NONE', 'WORKASPACE' ) ) ;
#11232 = ORIENTED_EDGE ( 'NONE', *, *, #19782, .F. ) ;
#11233 = B_SPLINE_CURVE_WITH_KNOTS ( 'NONE', 3,
 ( #14989, #10863, #12433, #19625, #21599, #8462, #19471, #22834, #14466, #5701, #21079, #11906, #10341, #20524, #3267, #9784, #18376, #27029, #3698, #12177, #25318, #7675, #27590, #27171, #1317, #16557, #1586, #5980, #23217, #16290, #3849, #8234, #10057, #3404 ),
 .UNSPECIFIED., .F., .F.,
 ( 4, 2, 2, 2, 2, 2, 2, 2, 2, 2, 2, 2, 2, 2, 2, 2, 4 ),
 ( 0.5000000000000000000, 0.5312500000000000000, 0.5625000000000000000, 0.5937500000000000000, 0.6250000000000001110, 0.6562500000000001110, 0.6875000000000001110, 0.7187500000000001110, 0.7500000000000000000, 0.7812500000000000000, 0.8125000000000001110, 0.8437500000000001110, 0.8750000000000001110, 0.9062500000000002220, 0.9375000000000001110, 0.9687500000000001110, 1.000000000000000000 ),
 .UNSPECIFIED. ) ;
#11234 = CARTESIAN_POINT ( 'NONE',  ( 0.4157391792961063204, 0.3323952789219082882, 0.3401574803149606252 ) ) ;
#11235 = CARTESIAN_POINT ( 'NONE',  ( -0.3145317858139328182, 0.4092783051644229841, 1.766732283464566899 ) ) ;
#11236 = CARTESIAN_POINT ( 'NONE',  ( 0.1649135259617042493, -0.4856708409200646281, 1.766732283464566899 ) ) ;
#11237 = DIRECTION ( 'NONE',  ( 0.000000000000000000, 0.000000000000000000, 1.000000000000000000 ) ) ;
#11238 = AXIS2_PLACEMENT_3D ( 'NONE', #16089, #15938, #24543 ) ;
#11239 = ORIENTED_EDGE ( 'NONE', *, *, #15878, .T. ) ;
#11240 = ORIENTED_EDGE ( 'NONE', *, *, #27737, .F. ) ;
#11241 = VECTOR ( 'NONE', #26043, 39.37007874015748143 ) ;
#11243 = CARTESIAN_POINT ( 'NONE',  ( -0.3644697409450256553, 0.09762295995070000010, -3.100567304031767168 ) ) ;
#11242 = CARTESIAN_POINT ( 'NONE',  ( -0.6476458834271923148, 0.1148891961916498478, 0.1461456498280682970 ) ) ;
#11245 = CARTESIAN_POINT ( 'NONE',  ( 0.06894484415077314909, -0.05111597790490109150, -0.4724409448818898127 ) ) ;
#11244 = ( REPRESENTATION_RELATIONSHIP ('NONE','NONE', #12434, #16232 ) REPRESENTATION_RELATIONSHIP_WITH_TRANSFORMATION ( #10427 )SHAPE_REPRESENTATION_RELATIONSHIP( ) ) ;
#11246 = CIRCLE ( 'NONE', #24774, 0.09143349766193348271 ) ;
#11247 = EDGE_LOOP ( 'NONE', ( #21822, #17189, #9787, #12456 ) ) ;
#11248 = CARTESIAN_POINT ( 'NONE',  ( -0.5382052855068000241, 0.4288813374988101890, 0.3401599409343964431 ) ) ;
#11249 = APPLICATION_CONTEXT ( 'automotive_design' ) ;
#11250 = DIRECTION ( 'NONE',  ( -0.2036417511401760472, 0.9790454724845840673, -1.198985000000000095E-16 ) ) ;
#11251 = ORIENTED_EDGE ( 'NONE', *, *, #11538, .F. ) ;
#11252 = CARTESIAN_POINT ( 'NONE',  ( -0.2521176338356522217, -0.2211428102655704220, 1.953740157480315043 ) ) ;
#11253 = ORIENTED_EDGE ( 'NONE', *, *, #1219, .T. ) ;
#11254 = EDGE_LOOP ( 'NONE', ( #27328, #5871, #12556, #15233, #16781, #13315 ) ) ;
#11255 = ADVANCED_FACE ( 'NONE', ( #25892 ), #4677, .F. ) ;
#11256 = DIRECTION ( 'NONE',  ( -1.000000000000000000, 0.000000000000000000, 0.000000000000000000 ) ) ;
#11257 = ORIENTED_EDGE ( 'NONE', *, *, #20611, .T. ) ;
#11258 = CARTESIAN_POINT ( 'NONE',  ( -0.1327952259510255528, -0.4954219348936245160, -1.550196850393701364 ) ) ;
#11259 = VERTEX_POINT ( 'NONE', #17274 ) ;
#11260 = EDGE_LOOP ( 'NONE', ( #25316, #20948 ) ) ;
#11261 = VERTEX_POINT ( 'NONE', #24182 ) ;
#11262 = CARTESIAN_POINT ( 'NONE',  ( 0.07874015748031495954, 0.1968503937007874127, -3.548228346456692162 ) ) ;
#11263 = EDGE_CURVE ( 'NONE', #20543, #8887, #26028, .T. ) ;
#11265 = CARTESIAN_POINT ( 'NONE',  ( -0.5177165354330708347, -0.4724409448818898127, -0.8182917201112815953 ) ) ;
#11266 = CARTESIAN_POINT ( 'NONE',  ( -0.2979095355689177493, -0.6203660015065670663, 0.3401574803149606252 ) ) ;
#11267 = CARTESIAN_POINT ( 'NONE',  ( 0.3872945158171015589, 4.827365162822171701E-17, -0.2204724409448818867 ) ) ;
#11268 = ORIENTED_EDGE ( 'NONE', *, *, #21213, .F. ) ;
#11269 = EDGE_CURVE ( 'NONE', #27077, #22659, #24948, .T. ) ;
#11270 = VECTOR ( 'NONE', #3000, 39.37007874015748143 ) ;
#11271 = CONICAL_SURFACE ( 'NONE', #14436, 0.3458446900868161200, 0.2407725888118960322 ) ;
#11272 = DIRECTION ( 'NONE',  ( 1.224646799147353207E-16, 1.000000000000000000, -0.000000000000000000 ) ) ;
#11273 = CARTESIAN_POINT ( 'NONE',  ( 0.1570220809524492389, -0.3184841198566451537, 1.953740157480315043 ) ) ;
#11274 = DIRECTION ( 'NONE',  ( 0.000000000000000000, 1.000000000000000000, 0.000000000000000000 ) ) ;
#11275 = CIRCLE ( 'NONE', #22162, 0.1771653543307086798 ) ;
#11276 = CARTESIAN_POINT ( 'NONE',  ( -0.3614376061968875287, -1.111631388898730588, -0.4004058270235824613 ) ) ;
#11277 = DIRECTION ( 'NONE',  ( 0.000000000000000000, 0.000000000000000000, -1.000000000000000000 ) ) ;
#11278 = DIRECTION ( 'NONE',  ( 0.000000000000000000, 1.000000000000000000, 0.000000000000000000 ) ) ;
#11279 = DIRECTION ( 'NONE',  ( -1.000000000000000000, 0.000000000000000000, 0.000000000000000000 ) ) ;
#11280 = FACE_OUTER_BOUND ( 'NONE', #27389, .T. ) ;
#11281 = ORIENTED_EDGE ( 'NONE', *, *, #19826, .T. ) ;
#11282 = DIRECTION ( 'NONE',  ( -0.000000000000000000, -0.000000000000000000, 1.000000000000000000 ) ) ;
#11283 = VECTOR ( 'NONE', #12756, 39.37007874015748143 ) ;
#11284 = CARTESIAN_POINT ( 'NONE',  ( 0.1516263115863346334, -0.4909405214979283838, 0.05579628926458630317 ) ) ;
#11285 = ORIENTED_EDGE ( 'NONE', *, *, #20791, .F. ) ;
#11286 = ORIENTED_EDGE ( 'NONE', *, *, #19746, .F. ) ;
#11287 = EDGE_CURVE ( 'NONE', #12667, #27484, #15760, .T. ) ;
#11288 = VECTOR ( 'NONE', #19329, 39.37007874015748143 ) ;
#11289 = DIRECTION ( 'NONE',  ( -1.000000000000000000, 0.000000000000000000, 0.000000000000000000 ) ) ;
#11290 = CARTESIAN_POINT ( 'NONE',  ( -0.3346456692913385988, 2.134256245050205639E-17, 1.973425196850393970 ) ) ;
#11291 = VERTEX_POINT ( 'NONE', #24040 ) ;
#11292 = CARTESIAN_POINT ( 'NONE',  ( 0.03607471876262466348, 0.5511811023622048555, 0.9399606299212598381 ) ) ;
#11293 = EDGE_CURVE ( 'NONE', #4526, #9781, #7822, .T. ) ;
#11294 = CARTESIAN_POINT ( 'NONE',  ( -0.3661417322834645272, -0.4724409448818898127, -0.8182917201112815953 ) ) ;
#11295 = ORIENTED_EDGE ( 'NONE', *, *, #4159, .T. ) ;
#11296 = CARTESIAN_POINT ( 'NONE',  ( 0.3268939675028499914, -0.1881330340946397728, 0.07637795275590551769 ) ) ;
#11297 = DIRECTION ( 'NONE',  ( 0.000000000000000000, 1.000000000000000000, 0.000000000000000000 ) ) ;
#11298 = CARTESIAN_POINT ( 'NONE',  ( -0.1870078740157480324, 0.8267716535433071723, 0.000000000000000000 ) ) ;
#11299 = FACE_OUTER_BOUND ( 'NONE', #18934, .T. ) ;
#11300 = CARTESIAN_POINT ( 'NONE',  ( 0.07874015748031495954, 0.1968503937007874127, -3.548228346456692162 ) ) ;
#11301 = DIRECTION ( 'NONE',  ( 0.000000000000000000, 1.000000000000000000, 0.000000000000000000 ) ) ;
#11302 = EDGE_CURVE ( 'NONE', #9249, #11890, #22245, .T. ) ;
#11303 = DIRECTION ( 'NONE',  ( -0.8660254037844388186, -0.4999999999999997780, 0.000000000000000000 ) ) ;
#11304 = EDGE_CURVE ( 'NONE', #17730, #8069, #24491, .T. ) ;
#11305 = CARTESIAN_POINT ( 'NONE',  ( 0.000000000000000000, 0.9055118110236221041, 0.000000000000000000 ) ) ;
#11306 = FACE_OUTER_BOUND ( 'NONE', #1631, .T. ) ;
#11307 = CARTESIAN_POINT ( 'NONE',  ( -0.5417097841048799101, -0.1839420097223198047, 0.9399606299212598381 ) ) ;
#11308 = DIRECTION ( 'NONE',  ( 0.000000000000000000, 1.000000000000000000, 0.000000000000000000 ) ) ;
#11309 = CARTESIAN_POINT ( 'NONE',  ( 0.1522836969735573143, 0.2938892803217905692, 0.3971963147566898167 ) ) ;
#11310 = EDGE_LOOP ( 'NONE', ( #26782, #13570, #21617, #25623 ) ) ;
#11311 = FACE_OUTER_BOUND ( 'NONE', #27357, .T. ) ;
#11312 = AXIS2_PLACEMENT_3D ( 'NONE', #25946, #7, #13487 ) ;
#11313 = ORIENTED_EDGE ( 'NONE', *, *, #27668, .T. ) ;
#11314 = CARTESIAN_POINT ( 'NONE',  ( -0.03349795313024241800, -0.5118110236220473341, -1.550196850393700920 ) ) ;
#11315 = DIRECTION ( 'NONE',  ( -1.000000000000000000, 0.000000000000000000, 0.000000000000000000 ) ) ;
#11316 = DIRECTION ( 'NONE',  ( 0.000000000000000000, 0.000000000000000000, -1.000000000000000000 ) ) ;
#11317 = EDGE_LOOP ( 'NONE', ( #6299, #22126, #12467, #18465 ) ) ;
#11318 = CARTESIAN_POINT ( 'NONE',  ( -0.4857079805365445146, 0.1648275707510890309, -1.550196850393700254 ) ) ;
#11319 = EDGE_CURVE ( 'NONE', #17345, #22917, #9594, .T. ) ;
#11320 = DIRECTION ( 'NONE',  ( 1.000000000000000000, 0.000000000000000000, 0.000000000000000000 ) ) ;
#11321 = ORIENTED_EDGE ( 'NONE', *, *, #2768, .T. ) ;
#11322 = EDGE_CURVE ( 'NONE', #11971, #25691, #3277, .T. ) ;
#11323 = PLANE ( 'NONE',  #26 ) ;
#11324 = VECTOR ( 'NONE', #25087, 39.37007874015748143 ) ;
#11325 = DIRECTION ( 'NONE',  ( 0.000000000000000000, 1.000000000000000000, 0.000000000000000000 ) ) ;
#11326 = CARTESIAN_POINT ( 'NONE',  ( 0.7874015748031325534, 0.2476103627152109743, -0.2796030453571548002 ) ) ;
#11327 = ORIENTED_EDGE ( 'NONE', *, *, #2422, .T. ) ;
#11328 = MECHANICAL_DESIGN_GEOMETRIC_PRESENTATION_REPRESENTATION (  '', ( #7735 ), #15842 ) ;
#11329 = TOROIDAL_SURFACE ( 'NONE', #1880, 0.4232283464566928832, 0.07677165354330708902 ) ;
#11330 = FACE_OUTER_BOUND ( 'NONE', #1660, .T. ) ;
#11331 = CARTESIAN_POINT ( 'NONE',  ( 0.03937007874015747977, 0.000000000000000000, 0.000000000000000000 ) ) ;
#11332 = ORIENTED_EDGE ( 'NONE', *, *, #7331, .F. ) ;
#11333 = DIRECTION ( 'NONE',  ( -0.000000000000000000, -0.000000000000000000, 1.000000000000000000 ) ) ;
#11334 = CARTESIAN_POINT ( 'NONE',  ( -0.2362204724409449064, 0.000000000000000000, 0.000000000000000000 ) ) ;
#11335 = CARTESIAN_POINT ( 'NONE',  ( 0.3001918266902036669, -0.3912931228432058872, -1.550196850393700920 ) ) ;
#11336 = CARTESIAN_POINT ( 'NONE',  ( -0.1477428134820414352, -0.4351030398461918081, -1.928289503579139641 ) ) ;
#11337 = EDGE_LOOP ( 'NONE', ( #268, #17619, #23146, #22248 ) ) ;
#11338 = CARTESIAN_POINT ( 'NONE',  ( 0.03607471876262465654, 0.5511811023622047445, 0.9202755905511811330 ) ) ;
#11339 = CARTESIAN_POINT ( 'NONE',  ( 0.000000000000000000, 0.000000000000000000, 0.2362204724409449064 ) ) ;
#11340 = DIRECTION ( 'NONE',  ( 0.000000000000000000, 0.000000000000000000, 1.000000000000000000 ) ) ;
#11341 = CARTESIAN_POINT ( 'NONE',  ( 0.2297883689023126064, 0.3979194638820598984, -1.928289503579157183 ) ) ;
#11342 = EDGE_CURVE ( 'NONE', #12052, #24279, #21796, .T. ) ;
#11343 = ORIENTED_EDGE ( 'NONE', *, *, #1377, .F. ) ;
#11344 = ORIENTED_EDGE ( 'NONE', *, *, #2784, .T. ) ;
#11345 = CARTESIAN_POINT ( 'NONE',  ( -4.821283464566928349E-18, 0.000000000000000000, -0.3779527559055118058 ) ) ;
#11346 = LINE ( 'NONE', #20382, #6561 ) ;
#11347 = CARTESIAN_POINT ( 'NONE',  ( 0.000000000000000000, 0.000000000000000000, 0.02362204724409448786 ) ) ;
#11348 = CARTESIAN_POINT ( 'NONE',  ( 0.2303471512294322787, -0.4798602677570401598, 0.1322834645669291320 ) ) ;
#11349 = CIRCLE ( 'NONE', #20386, 0.1771653543307086798 ) ;
#11350 = CARTESIAN_POINT ( 'NONE',  ( -0.0006737210091418004447, 0.6438792636756986987, 0.1183902030408860162 ) ) ;
#11351 = EDGE_CURVE ( 'NONE', #14153, #20978, #27698, .T. ) ;
#11352 = ADVANCED_FACE ( 'NONE', ( #17096 ), #15495, .F. ) ;
#11353 = CARTESIAN_POINT ( 'NONE',  ( 0.4771018889076559244, 0.3804760601893846794, 0.2362204724409449064 ) ) ;
#11354 = CYLINDRICAL_SURFACE ( 'NONE', #8250, 0.1181102362204720091 ) ;
#11355 = VERTEX_POINT ( 'NONE', #6363 ) ;
#11356 = CARTESIAN_POINT ( 'NONE',  ( -0.6562077975700097987, -7.454212598425196280E-14, -0.07874015748031495954 ) ) ;
#11357 = ORIENTED_EDGE ( 'NONE', *, *, #12974, .T. ) ;
#11358 = CARTESIAN_POINT ( 'NONE',  ( 0.2427018018350767803, 0.2887032559529629783, 0.07637630750536809898 ) ) ;
#11359 = VERTEX_POINT ( 'NONE', #3965 ) ;
#11360 = CARTESIAN_POINT ( 'NONE',  ( 0.1516263115863346334, -0.1971492568089271424, 0.4530651079966787620 ) ) ;
#11361 = DIRECTION ( 'NONE',  ( -0.8660254037844385966, -0.5000000000000002220, 0.000000000000000000 ) ) ;
#11362 = DIRECTION ( 'NONE',  ( 1.000000000000000000, 0.000000000000000000, 0.000000000000000000 ) ) ;
#11363 = CIRCLE ( 'NONE', #19474, 0.07677362204724408334 ) ;
#11364 = CARTESIAN_POINT ( 'NONE',  ( 0.4219236230596370985, -0.1431838228103867738, -1.934055118110236116 ) ) ;
#11365 = CARTESIAN_POINT ( 'NONE',  ( 0.3267488823401750175, 0.1886891683788910201, -3.100567304031762284 ) ) ;
#11366 = DIRECTION ( 'NONE',  ( 0.000000000000000000, 0.000000000000000000, 1.000000000000000000 ) ) ;
#11367 = CARTESIAN_POINT ( 'NONE',  ( 0.000000000000000000, 0.000000000000000000, -0.2204724409448818867 ) ) ;
#11368 = VERTEX_POINT ( 'NONE', #21200 ) ;
#11369 = CARTESIAN_POINT ( 'NONE',  ( -0.3935368318888681771, -0.3024344094364740387, -1.569881889763780070 ) ) ;
#11370 = AXIS2_PLACEMENT_3D ( 'NONE', #20240, #23472, #14730 ) ;
#11371 = AXIS2_PLACEMENT_3D ( 'NONE', #4183, #14371, #16473 ) ;
#11372 = EDGE_CURVE ( 'NONE', #19029, #16219, #19485, .T. ) ;
#11373 = VERTEX_POINT ( 'NONE', #24272 ) ;
#11374 = LINE ( 'NONE', #4732, #12398 ) ;
#11375 = CARTESIAN_POINT ( 'NONE',  ( -0.6299212598425196763, -0.4526313213353582721, 0.9943460912301771426 ) ) ;
#11376 = CARTESIAN_POINT ( 'NONE',  ( -0.6299212598425196763, -0.6348133144914134274, 0.8891632684400255782 ) ) ;
#11377 = CARTESIAN_POINT ( 'NONE',  ( -0.1649135259616916205, -0.4856708409200665155, 1.747047244094488194 ) ) ;
#11378 = ADVANCED_FACE ( 'NONE', ( #6501 ), #10064, .F. ) ;
#11379 = DIRECTION ( 'NONE',  ( 0.000000000000000000, 0.000000000000000000, 1.000000000000000000 ) ) ;
#11380 = AXIS2_PLACEMENT_3D ( 'NONE', #25117, #7612, #22580 ) ;
#11381 = CONICAL_SURFACE ( 'NONE', #21326, 0.3066721922917531873, 0.5845243560369969282 ) ;
#11382 = CARTESIAN_POINT ( 'NONE',  ( 0.2807137536170455361, -0.2462256503455606815, -3.115157480314960647 ) ) ;
#11383 = EDGE_CURVE ( 'NONE', #17093, #5287, #13393, .T. ) ;
#11384 = DIRECTION ( 'NONE',  ( -0.6427876096865390299, 0.7660444431189783465, 0.000000000000000000 ) ) ;
#11385 = CARTESIAN_POINT ( 'NONE',  ( 0.000000000000000000, 0.1574803148899641958, 0.000000000000000000 ) ) ;
#11386 = EDGE_LOOP ( 'NONE', ( #9114, #13912, #4514, #14867 ) ) ;
#11387 = CARTESIAN_POINT ( 'NONE',  ( -0.3346456692913385988, 0.02190250779246044610, 1.953740157480315043 ) ) ;
#11388 = ORIENTED_EDGE ( 'NONE', *, *, #16418, .T. ) ;
#11389 = EDGE_LOOP ( 'NONE', ( #16582, #5201, #22031, #25192, #23159 ) ) ;
#11390 = CONICAL_SURFACE ( 'NONE', #13202, 0.6942509683549429322, 0.2617993875000015902 ) ;
#11391 = VERTEX_POINT ( 'NONE', #2312 ) ;
#11392 = DIRECTION ( 'NONE',  ( -0.000000000000000000, -0.000000000000000000, -1.000000000000000000 ) ) ;
#11393 = ORIENTED_EDGE ( 'NONE', *, *, #25719, .F. ) ;
#11394 = ORIENTED_EDGE ( 'NONE', *, *, #3074, .T. ) ;
#11395 = CARTESIAN_POINT ( 'NONE',  ( 0.03962771305384435450, 0.1968503937007874127, -3.617038702773737402 ) ) ;
#11396 = CARTESIAN_POINT ( 'NONE',  ( -8.632637795275590524E-16, -0.8267716535433071723, 0.000000000000000000 ) ) ;
#11397 = CARTESIAN_POINT ( 'NONE',  ( 0.06294778803456628491, 0.1968503937007874127, -3.224226213012447051 ) ) ;
#11398 = CARTESIAN_POINT ( 'NONE',  ( 0.6933858814654041414, 0.7755322313789173583, -0.02322279011146228048 ) ) ;
#11399 = AXIS2_PLACEMENT_3D ( 'NONE', #16563, #27312, #5270 ) ;
#11400 = CARTESIAN_POINT ( 'NONE',  ( -0.02559055118110236185, 0.8267716535433071723, 0.000000000000000000 ) ) ;
#11401 = AXIS2_PLACEMENT_3D ( 'NONE', #19116, #10211, #25624 ) ;
#11402 = CARTESIAN_POINT ( 'NONE',  ( 0.09842519685039370636, 0.2165354330708661457, -3.272637795275590733 ) ) ;
#11403 = AXIS2_PLACEMENT_3D ( 'NONE', #23848, #2349, #21991 ) ;
#11404 = DIRECTION ( 'NONE',  ( -1.000000000000000000, 0.000000000000000000, 0.000000000000000000 ) ) ;
#11405 = ADVANCED_FACE ( 'NONE', ( #1763 ), #10657, .F. ) ;
#11406 = AXIS2_PLACEMENT_3D ( 'NONE', #20481, #7633, #20762 ) ;
#11407 = CARTESIAN_POINT ( 'NONE',  ( 0.3722026523000413478, 4.558167867734008572E-17, -0.2204724409448818867 ) ) ;
#11408 = DIRECTION ( 'NONE',  ( 1.000000000000000000, 0.000000000000000000, 0.000000000000000000 ) ) ;
#11409 = CARTESIAN_POINT ( 'NONE',  ( 0.4010740433761567081, 4.911740434416970370E-17, -0.2342519685039370358 ) ) ;
#11410 = DIRECTION ( 'NONE',  ( -0.2225209339563143096, 0.9749279121818237304, 0.000000000000000000 ) ) ;
#11411 = ADVANCED_FACE ( 'NONE', ( #22084, #758 ), #9754, .T. ) ;
#11412 = CARTESIAN_POINT ( 'NONE',  ( 0.5118110236220472231, 0.03349795313260757468, 1.766732283464566899 ) ) ;
#11413 = CARTESIAN_POINT ( 'NONE',  ( -0.002724751885584173784, -0.1704774416898503786, -0.09842519685039387289 ) ) ;
#11414 = ORIENTED_EDGE ( 'NONE', *, *, #19334, .T. ) ;
#11415 = DIRECTION ( 'NONE',  ( -0.2036417511401758251, -0.4895227362422921447, -0.8478782506317885659 ) ) ;
#11416 = CIRCLE ( 'NONE', #27675, 1.377952755905512472 ) ;
#11417 = ORIENTED_EDGE ( 'NONE', *, *, #25810, .F. ) ;
#11418 = EDGE_LOOP ( 'NONE', ( #11948, #27000, #19212, #20771 ) ) ;
#11419 = CIRCLE ( 'NONE', #11868, 0.1673228346456692994 ) ;
#11420 = CARTESIAN_POINT ( 'NONE',  ( 0.5118110236220472231, 6.267877318470705905E-17, -0.2618110236220472231 ) ) ;
#11421 = CARTESIAN_POINT ( 'NONE',  ( 0.5869493968219645641, 0.4267795243146149664, 0.000000000000000000 ) ) ;
#11422 = VERTEX_POINT ( 'NONE', #728 ) ;
#11423 = CARTESIAN_POINT ( 'NONE',  ( -0.2442565704126459791, -0.4954197419817803483, 0.9399606299212598381 ) ) ;
#11424 = CIRCLE ( 'NONE', #27227, 0.4986013261500205074 ) ;
#11425 = VERTEX_POINT ( 'NONE', #8321 ) ;
#11426 = LINE ( 'NONE', #13405, #25714 ) ;
#11427 = ADVANCED_FACE ( 'NONE', ( #8590, #25121, #12554, #6342, #16653, #1672, #1813, #25263, #14971, #23018 ), #14704, .T. ) ;
#11428 = DIRECTION ( 'NONE',  ( 1.000000000000000000, 0.000000000000000000, 0.000000000000000000 ) ) ;
#11429 = CARTESIAN_POINT ( 'NONE',  ( 0.4932478747986535628, 0.08657132889677619791, 0.2574819596263889787 ) ) ;
#11430 = CIRCLE ( 'NONE', #27233, 0.09143349766193348271 ) ;
#11431 = CARTESIAN_POINT ( 'NONE',  ( 0.6106000000000000316, -1.355930314960630041E-19, 0.000000000000000000 ) ) ;
#11432 = CARTESIAN_POINT ( 'NONE',  ( 0.3905379133858267737, 0.5610236220472440971, 0.000000000000000000 ) ) ;
#11433 = CARTESIAN_POINT ( 'NONE',  ( -1.452994488188976472E-16, 0.5905905511811023745, -3.548228346456693050 ) ) ;
#11434 = CARTESIAN_POINT ( 'NONE',  ( -0.4021324607134745821, 0.3215300179743675324, 0.3251195115596967611 ) ) ;
#11435 = CARTESIAN_POINT ( 'NONE',  ( -0.3007905576423960392, -0.1482986320106512990, 1.953740157480315043 ) ) ;
#11436 = DIRECTION ( 'NONE',  ( 0.000000000000000000, 0.000000000000000000, -1.000000000000000000 ) ) ;
#11437 = CLOSED_SHELL ( 'NONE', ( #10710, #6575, #25133, #27475, #21815, #6487, #27483, #4397, #7234, #16832, #9544, #18190, #27800, #6281, #25277, #13325, #19806, #11529, #18769, #7339, #11754, #9724, #12785, #23206, #20744, #2956, #13353, #19719, #11473, #18635, #14007, #11541, #20961, #11255, #27709, #8056, #18607 ) ) ;
#11438 = DIRECTION ( 'NONE',  ( 1.000000000000000000, 0.000000000000000000, 0.000000000000000000 ) ) ;
#11439 = CARTESIAN_POINT ( 'NONE',  ( 0.1518453844022533417, 0.4909359254662000183, -0.05583672883938756160 ) ) ;
#11440 = EDGE_CURVE ( 'NONE', #10350, #19648, #950, .T. ) ;
#11441 = FACE_OUTER_BOUND ( 'NONE', #4334, .T. ) ;
#11442 = EDGE_CURVE ( 'NONE', #4513, #11989, #23310, .T. ) ;
#11443 = CARTESIAN_POINT ( 'NONE',  ( -0.5118110236220472231, -0.06699590632655398614, 1.766732283464566677 ) ) ;
#11444 = CARTESIAN_POINT ( 'NONE',  ( -0.09842519685039370636, 0.2165354330708661457, -3.548228346456693050 ) ) ;
#11445 = DIRECTION ( 'NONE',  ( 0.000000000000000000, 0.000000000000000000, -1.000000000000000000 ) ) ;
#11446 = EDGE_CURVE ( 'NONE', #4298, #21302, #596, .T. ) ;
#11447 = FACE_OUTER_BOUND ( 'NONE', #27179, .T. ) ;
#11448 = VECTOR ( 'NONE', #20797, 39.37007874015748854 ) ;
#11449 = B_SPLINE_CURVE_WITH_KNOTS ( 'NONE', 3,
 ( #3503, #5359, #23166, #22592, #18762, #27122 ),
 .UNSPECIFIED., .F., .F.,
 ( 4, 2, 4 ),
 ( 0.3108507187342950395, 0.3125269569790680158, 0.3142031952238389936 ),
 .UNSPECIFIED. ) ;
#11450 = AXIS2_PLACEMENT_3D ( 'NONE', #4763, #11272, #19891 ) ;
#11451 = ADVANCED_FACE ( 'NONE', ( #23586 ), #18893, .T. ) ;
#11452 = VERTEX_POINT ( 'NONE', #23450 ) ;
#11453 = DIRECTION ( 'NONE',  ( 0.000000000000000000, 0.000000000000000000, 1.000000000000000000 ) ) ;
#11454 = DIRECTION ( 'NONE',  ( -0.4999999999999998890, -0.8660254037844388186, 0.000000000000000000 ) ) ;
#11455 = VERTEX_POINT ( 'NONE', #16793 ) ;
#11456 = DIRECTION ( 'NONE',  ( 0.000000000000000000, 1.000000000000000000, 0.000000000000000000 ) ) ;
#11457 = ORIENTED_EDGE ( 'NONE', *, *, #22449, .F. ) ;
#11458 = CIRCLE ( 'NONE', #8748, 1.288838582677165112 ) ;
#11459 = CARTESIAN_POINT ( 'NONE',  ( 0.000000000000000000, 0.000000000000000000, 0.04842519685039370358 ) ) ;
#11460 = ORIENTED_EDGE ( 'NONE', *, *, #18237, .T. ) ;
#11461 = EDGE_CURVE ( 'NONE', #9428, #13016, #11416, .T. ) ;
#11462 = CARTESIAN_POINT ( 'NONE',  ( 0.1279527559055118058, -0.7874015748031496509, 9.642888182262624280E-17 ) ) ;
#11463 = B_SPLINE_CURVE_WITH_KNOTS ( 'NONE', 3,
 ( #538, #3184, #26642, #1097, #13380, #7297, #22418, #20016, #7164, #22005, #16064, #18143, #15916, #11397, #2638, #13799, #26787, #24656 ),
 .UNSPECIFIED., .F., .F.,
 ( 4, 2, 2, 2, 2, 2, 2, 2, 4 ),
 ( 0.000000000000000000, 0.1250000000000000000, 0.2500000000000000000, 0.3750000000000000000, 0.5000000000000000000, 0.6250000000000000000, 0.7500000000000000000, 0.8750000000000000000, 1.000000000000000000 ),
 .UNSPECIFIED. ) ;
#11464 = DIRECTION ( 'NONE',  ( 1.000000000000000000, 0.000000000000000000, 0.000000000000000000 ) ) ;
#11465 = AXIS2_PLACEMENT_3D ( 'NONE', #10731, #44, #8606 ) ;
#11466 = CARTESIAN_POINT ( 'NONE',  ( -0.3661417322834645272, 0.9448818897637796255, 0.1771653543307086520 ) ) ;
#11467 = DIRECTION ( 'NONE',  ( -0.000000000000000000, -0.000000000000000000, -1.000000000000000000 ) ) ;
#11468 = TOROIDAL_SURFACE ( 'NONE', #6095, 0.4980314960629921295, 0.01377952755905511792 ) ;
#11469 = ORIENTED_EDGE ( 'NONE', *, *, #22166, .F. ) ;
#11470 = CARTESIAN_POINT ( 'NONE',  ( 0.09842519685039360922, 0.2991866959364321565, -3.554782022675774922 ) ) ;
#11471 = CARTESIAN_POINT ( 'NONE',  ( -0.5118110236220473341, 0.000000000000000000, -1.550196850393700920 ) ) ;
#11472 = CARTESIAN_POINT ( 'NONE',  ( -0.2796934465393772773, -0.3645739570812616681, -1.928289503579163178 ) ) ;
#11473 = ADVANCED_FACE ( 'NONE', ( #12824 ), #24115, .F. ) ;
#11474 = CARTESIAN_POINT ( 'NONE',  ( 3.606039370078740678E-16, -1.259842519685039353, 7.714310545810098438E-17 ) ) ;
#11475 = DIRECTION ( 'NONE',  ( 1.000000000000000000, 0.000000000000000000, 0.000000000000000000 ) ) ;
#11476 = DIRECTION ( 'NONE',  ( 0.000000000000000000, 0.000000000000000000, -1.000000000000000000 ) ) ;
#11477 = CARTESIAN_POINT ( 'NONE',  ( 0.3715251363271980245, 0.06498290224717499786, 0.1992125984251968684 ) ) ;
#11478 = ADVANCED_FACE ( 'NONE', ( #13371 ), #17478, .F. ) ;
#11479 = AXIS2_PLACEMENT_3D ( 'NONE', #13389, #19756, #9412 ) ;
#11480 = CARTESIAN_POINT ( 'NONE',  ( -0.3707612262532960501, 0.3252100150720461658, -1.569881889763779625 ) ) ;
#11481 = ADVANCED_FACE ( 'NONE', ( #8726 ), #5081, .T. ) ;
#11482 = CARTESIAN_POINT ( 'NONE',  ( -0.6562077975700453258, 1.655117322834645733E-14, -0.2362204724409449064 ) ) ;
#11483 = CARTESIAN_POINT ( 'NONE',  ( 0.000000000000000000, 0.000000000000000000, -0.2952755905511805778 ) ) ;
#11484 = DIRECTION ( 'NONE',  ( -0.7071067818211409506, -0.7071067805519539728, 0.000000000000000000 ) ) ;
#11485 = CARTESIAN_POINT ( 'NONE',  ( -0.5731455175601024576, -0.3301167833454110578, 0.1926811207745849075 ) ) ;
#11486 = AXIS2_PLACEMENT_3D ( 'NONE', #14284, #22895, #12143 ) ;
#11487 = ( NAMED_UNIT ( * ) SI_UNIT ( $, .STERADIAN. ) SOLID_ANGLE_UNIT ( ) ) ;
#11488 = AXIS2_PLACEMENT_3D ( 'NONE', #3609, #20153, #954 ) ;
#11489 = CARTESIAN_POINT ( 'NONE',  ( 0.4165721057576322606, 0.3313508221749649763, 0.3401574803149606252 ) ) ;
#11490 = ORIENTED_EDGE ( 'NONE', *, *, #21044, .F. ) ;
#11491 = CARTESIAN_POINT ( 'NONE',  ( -0.7874015748031496509, 0.3648237195092146057, -0.1496552535541220419 ) ) ;
#11492 = ORIENTED_EDGE ( 'NONE', *, *, #18272, .T. ) ;
#11493 = ORIENTED_EDGE ( 'NONE', *, *, #10737, .F. ) ;
#11494 = CARTESIAN_POINT ( 'NONE',  ( 0.4527559054764770385, 0.02963280468032115228, -1.934055118110236338 ) ) ;
#11495 = LINE ( 'NONE', #20674, #3537 ) ;
#11496 = CARTESIAN_POINT ( 'NONE',  ( 0.5491102354215032788, -0.3162573801172474663, 0.2481708550950798842 ) ) ;
#11497 = CARTESIAN_POINT ( 'NONE',  ( 0.1512834625131516675, -0.2841833823079704668, -0.3983296490053409022 ) ) ;
#11498 = FACE_OUTER_BOUND ( 'NONE', #1760, .T. ) ;
#11499 = CARTESIAN_POINT ( 'NONE',  ( 0.1490609433537086470, 0.2308937649799950309, 0.4193412272900834958 ) ) ;
#11500 = CARTESIAN_POINT ( 'NONE',  ( 0.000000000000000000, 0.000000000000000000, -1.092739370078740131E-17 ) ) ;
#11501 = CIRCLE ( 'NONE', #8356, 0.4803149606299212393 ) ;
#11502 = CARTESIAN_POINT ( 'NONE',  ( 0.3998447049182496382, 0.4754871227240771714, 0.09685039370078740717 ) ) ;
#11503 = DIRECTION ( 'NONE',  ( 0.000000000000000000, 1.000000000000000000, 0.000000000000000000 ) ) ;
#11504 = CARTESIAN_POINT ( 'NONE',  ( 0.03008364706454716778, -0.1136516277932324709, -0.1968503937007874127 ) ) ;
#11505 = CARTESIAN_POINT ( 'NONE',  ( -0.02464264302293858039, -0.3765118517642103702, -3.100567304031763172 ) ) ;
#11506 = FACE_OUTER_BOUND ( 'NONE', #22818, .T. ) ;
#11507 = FACE_OUTER_BOUND ( 'NONE', #3068, .T. ) ;
#11508 = VERTEX_POINT ( 'NONE', #2631 ) ;
#11509 = CIRCLE ( 'NONE', #27307, 0.8031496062992127261 ) ;
#11510 = CIRCLE ( 'NONE', #25966, 0.03937007874015751446 ) ;
#11511 = PRODUCT_CONTEXT ( 'NONE', #14882, 'mechanical' ) ;
#11512 = ORIENTED_EDGE ( 'NONE', *, *, #17874, .F. ) ;
#11513 = ORIENTED_EDGE ( 'NONE', *, *, #15906, .T. ) ;
#11514 = CARTESIAN_POINT ( 'NONE',  ( 0.3606190329934327310, 0.4297690281277732338, 0.1771653543307086520 ) ) ;
#11515 = DIRECTION ( 'NONE',  ( 0.000000000000000000, 0.000000000000000000, 1.000000000000000000 ) ) ;
#11516 = CARTESIAN_POINT ( 'NONE',  ( 0.5118110236220472231, -0.03349795313260760937, 1.766732283464566899 ) ) ;
#11517 = CIRCLE ( 'NONE', #19646, 0.3464566929133857665 ) ;
#11518 = ORIENTED_EDGE ( 'NONE', *, *, #26098, .F. ) ;
#11519 = CARTESIAN_POINT ( 'NONE',  ( -0.2807137536170348779, -0.2462256503456018430, -3.115157480314960647 ) ) ;
#11520 = CARTESIAN_POINT ( 'NONE',  ( -0.7874015748031496509, 0.3648237195092146057, -0.1496552535541220419 ) ) ;
#11521 = CARTESIAN_POINT ( 'NONE',  ( -0.2165354330708661457, -1.112204724409448842, 0.000000000000000000 ) ) ;
#11522 = ORIENTED_EDGE ( 'NONE', *, *, #3428, .F. ) ;
#11523 = ORIENTED_EDGE ( 'NONE', *, *, #211, .T. ) ;
#11524 = FACE_OUTER_BOUND ( 'NONE', #18595, .T. ) ;
#11525 = ORIENTED_EDGE ( 'NONE', *, *, #21299, .F. ) ;
#11526 = DIRECTION ( 'NONE',  ( -0.000000000000000000, -1.000000000000000000, -0.000000000000000000 ) ) ;
#11527 = ORIENTED_EDGE ( 'NONE', *, *, #16150, .T. ) ;
#11528 = VERTEX_POINT ( 'NONE', #26230 ) ;
#11529 = ADVANCED_FACE ( 'NONE', ( #25828 ), #22129, .T. ) ;
#11530 = CYLINDRICAL_SURFACE ( 'NONE', #26314, 0.5007874015748031704 ) ;
#11531 = ADVANCED_FACE ( 'NONE', ( #4614 ), #27222, .T. ) ;
#11532 = CONICAL_SURFACE ( 'NONE', #15174, 0.4526932812344527379, 0.1178097243749990780 ) ;
#11533 = CARTESIAN_POINT ( 'NONE',  ( 0.2083728861314909642, 0.5965552328248759917, 0.1367407604580403446 ) ) ;
#11534 = PRODUCT_RELATED_PRODUCT_CATEGORY ( 'part', '', ( #3449 ) ) ;
#11535 = DIRECTION ( 'NONE',  ( 0.000000000000000000, 0.000000000000000000, 1.000000000000000000 ) ) ;
#11536 = CARTESIAN_POINT ( 'NONE',  ( 0.000000000000000000, 0.4724409448818898127, 0.000000000000000000 ) ) ;
#11537 = FACE_OUTER_BOUND ( 'NONE', #26626, .T. ) ;
#11538 = EDGE_CURVE ( 'NONE', #1564, #2742, #13211, .T. ) ;
#11539 = AXIS2_PLACEMENT_3D ( 'NONE', #21564, #25242, #23428 ) ;
#11540 = CARTESIAN_POINT ( 'NONE',  ( 0.5981657849660177995, -0.4807043897637795493, 5.886929133858268250E-17 ) ) ;
#11541 = ADVANCED_FACE ( 'NONE', ( #2355 ), #9122, .F. ) ;
#11542 = CARTESIAN_POINT ( 'NONE',  ( -0.2676050456844304426, -0.2056553984168022764, 1.973425196850394414 ) ) ;
#11543 = CARTESIAN_POINT ( 'NONE',  ( -0.6864238947227671028, -0.1574599019768544161, 0.1443310008632313346 ) ) ;
#11544 = CARTESIAN_POINT ( 'NONE',  ( 0.000000000000000000, 0.000000000000000000, -1.092739370078740131E-17 ) ) ;
#11545 = DIRECTION ( 'NONE',  ( 0.000000000000000000, 0.000000000000000000, 1.000000000000000000 ) ) ;
#11546 = AXIS2_PLACEMENT_3D ( 'NONE', #7496, #27418, #16395 ) ;
#11547 = DIRECTION ( 'NONE',  ( 0.000000000000000000, 0.000000000000000000, -1.000000000000000000 ) ) ;
#11548 = CARTESIAN_POINT ( 'NONE',  ( -0.5280699926563169333, 0.06957181182499308503, 1.747047244094488194 ) ) ;
#11549 = ORIENTED_EDGE ( 'NONE', *, *, #26249, .F. ) ;
#11550 = AXIS2_PLACEMENT_3D ( 'NONE', #16861, #19103, #21235 ) ;
#11551 = ORIENTED_EDGE ( 'NONE', *, *, #9655, .F. ) ;
#11552 = DIRECTION ( 'NONE',  ( -0.2588190449580413666, 3.169619149662402932E-17, 0.9659258263277814560 ) ) ;
#11553 = LINE ( 'NONE', #3203, #8736 ) ;
#11554 = ( NAMED_UNIT ( * ) PLANE_ANGLE_UNIT ( ) SI_UNIT ( $, .RADIAN. ) ) ;
#11555 = ORIENTED_EDGE ( 'NONE', *, *, #24176, .F. ) ;
#11556 = CARTESIAN_POINT ( 'NONE',  ( -0.4063220079890811354, -0.2348123150948578930, 0.07637549214372835182 ) ) ;
#11557 = ORIENTED_EDGE ( 'NONE', *, *, #1471, .F. ) ;
#11558 = CARTESIAN_POINT ( 'NONE',  ( -0.3912931228432153796, -0.3001918266902245391, -1.569881889763779625 ) ) ;
#11559 = CARTESIAN_POINT ( 'NONE',  ( -0.3713448905834433322, 0.06600512665679449109, 0.07637795275590551769 ) ) ;
#11560 = ORIENTED_EDGE ( 'NONE', *, *, #20508, .T. ) ;
#11561 = CARTESIAN_POINT ( 'NONE',  ( 0.3642352168757231889, -0.4152525734085952269, 0.9399606299212598381 ) ) ;
#11562 = ORIENTED_EDGE ( 'NONE', *, *, #12383, .F. ) ;
#11563 = DIRECTION ( 'NONE',  ( 0.000000000000000000, 1.000000000000000000, 0.000000000000000000 ) ) ;
#11564 = DIRECTION ( 'NONE',  ( 1.000000000000000000, 0.000000000000000000, 0.000000000000000000 ) ) ;
#11565 = PRODUCT_DEFINITION_FORMATION_WITH_SPECIFIED_SOURCE ( 'ANY', '', #24947, .NOT_KNOWN. ) ;
#11566 = CIRCLE ( 'NONE', #2978, 0.07677362204724408334 ) ;
#11567 = CARTESIAN_POINT ( 'NONE',  ( 0.1522836969735573143, 0.4909267390297480382, -0.05591742528025173131 ) ) ;
#11568 = EDGE_CURVE ( 'NONE', #5635, #18611, #10846, .T. ) ;
#11569 = CARTESIAN_POINT ( 'NONE',  ( 0.003937007874015826907, 8.142711329854796413E-18, 0.1023622047244094474 ) ) ;
#11570 = DIRECTION ( 'NONE',  ( -1.000000000000000000, 0.000000000000000000, 0.000000000000000000 ) ) ;
#11571 = EDGE_CURVE ( 'NONE', #18321, #23663, #6618, .T. ) ;
#11572 = AXIS2_PLACEMENT_3D ( 'NONE', #26391, #4922, #434 ) ;
#11573 = FACE_OUTER_BOUND ( 'NONE', #18417, .T. ) ;
#11574 = CARTESIAN_POINT ( 'NONE',  ( 0.06894484415258525511, 0.05111597790624471116, -0.4724409448841456749 ) ) ;
#11575 = CARTESIAN_POINT ( 'NONE',  ( -0.1247869790649115962, -0.3443449117941754234, 0.08455817588007014107 ) ) ;
#11576 = EDGE_CURVE ( 'NONE', #19099, #26373, #5656, .T. ) ;
#11577 = CARTESIAN_POINT ( 'NONE',  ( -0.2521176338356522217, -0.2211428102655704220, 1.953740157480315043 ) ) ;
#11578 = UNCERTAINTY_MEASURE_WITH_UNIT (LENGTH_MEASURE( 1.000000000000000082E-05 ), #21537, 'distance_accuracy_value', 'NONE') ;
#11579 = ORIENTED_EDGE ( 'NONE', *, *, #3879, .F. ) ;
#11580 = CARTESIAN_POINT ( 'NONE',  ( 0.5869493968219645641, -0.2133897621573078718, -0.3696019098714952711 ) ) ;
#11581 = CARTESIAN_POINT ( 'NONE',  ( -0.3209354104561039089, 0.3834063931590963037, 0.1259302777217432279 ) ) ;
#11582 = DIRECTION ( 'NONE',  ( -0.7071067811865480168, 0.7071067811865470176, 0.000000000000000000 ) ) ;
#11583 = CARTESIAN_POINT ( 'NONE',  ( -1.197070535079588716, 0.07874015748031491790, 1.197070535079588716 ) ) ;
#11584 = DIRECTION ( 'NONE',  ( -1.000000000000000000, 0.000000000000000000, 0.000000000000000000 ) ) ;
#11585 = DIRECTION ( 'NONE',  ( 0.000000000000000000, -1.000000000000000000, 0.000000000000000000 ) ) ;
#11586 = CARTESIAN_POINT ( 'NONE',  ( -0.2066929133858267931, 0.000000000000000000, 0.000000000000000000 ) ) ;
#11587 = ORIENTED_EDGE ( 'NONE', *, *, #11780, .T. ) ;
#11588 = AXIS2_PLACEMENT_3D ( 'NONE', #5229, #3665, #7923 ) ;
#11589 = ORIENTED_EDGE ( 'NONE', *, *, #3755, .T. ) ;
#11590 = CARTESIAN_POINT ( 'NONE',  ( 0.2952755905511810774, -3.755651186670777132E-17, -0.07578740157480315376 ) ) ;
#11591 = CARTESIAN_POINT ( 'NONE',  ( 0.1525037638700916243, -0.2314035372547590674, -0.4381595109572583580 ) ) ;
#11592 = EDGE_LOOP ( 'NONE', ( #7743, #801, #27491, #1286 ) ) ;
#11593 = DIRECTION ( 'NONE',  ( 1.000000000000000000, 0.000000000000000000, 0.000000000000000000 ) ) ;
#11594 = ORIENTED_EDGE ( 'NONE', *, *, #27605, .F. ) ;
#11595 = EDGE_LOOP ( 'NONE', ( #17928, #17734 ) ) ;
#11596 = EDGE_CURVE ( 'NONE', #11793, #2049, #6757, .T. ) ;
#11597 = CARTESIAN_POINT ( 'NONE',  ( -0.2243259791918627288, -0.6183223858019056829, 0.1461456498332554532 ) ) ;
#11598 = CARTESIAN_POINT ( 'NONE',  ( 0.6175000359513720394, 0.7947887377729331293, -0.2396602654345149352 ) ) ;
#11599 = EDGE_CURVE ( 'NONE', #8441, #8220, #287, .T. ) ;
#11600 = B_SPLINE_CURVE_WITH_KNOTS ( 'NONE', 3,
 ( #26410, #451, #2408, #11168 ),
 .UNSPECIFIED., .F., .F.,
 ( 4, 4 ),
 ( 0.2376120521391529850, 0.2390783382518553157 ),
 .UNSPECIFIED. ) ;
#11601 = DIRECTION ( 'NONE',  ( -0.000000000000000000, -1.000000000000000000, -0.000000000000000000 ) ) ;
#11602 = ORIENTED_EDGE ( 'NONE', *, *, #12114, .F. ) ;
#11603 = AXIS2_PLACEMENT_3D ( 'NONE', #1188, #7816, #27033 ) ;
#11604 = VERTEX_POINT ( 'NONE', #21588 ) ;
#11605 = AXIS2_PLACEMENT_3D ( 'NONE', #23955, #4588, #26755 ) ;
#11606 = CARTESIAN_POINT ( 'NONE',  ( -0.2904160862623674788, 0.1677079028045369846, 1.973425196850393970 ) ) ;
#11607 = CARTESIAN_POINT ( 'NONE',  ( 0.2466292688015316592, -0.4270824798167792147, -1.550196850393700920 ) ) ;
#11608 = EDGE_CURVE ( 'NONE', #5530, #18462, #1484, .T. ) ;
#11609 = CARTESIAN_POINT ( 'NONE',  ( -0.3715251363271980245, 0.06498290224717540031, 0.07637795275590551769 ) ) ;
#11610 = AXIS2_PLACEMENT_3D ( 'NONE', #4982, #24606, #16153 ) ;
#11611 = DIRECTION ( 'NONE',  ( 0.000000000000000000, 0.000000000000000000, 1.000000000000000000 ) ) ;
#11612 = DIRECTION ( 'NONE',  ( 0.000000000000000000, 0.000000000000000000, -1.000000000000000000 ) ) ;
#11613 = CARTESIAN_POINT ( 'NONE',  ( 0.3714054139060134485, 0.06566393819133227450, 0.1992150590373740204 ) ) ;
#11614 = CARTESIAN_POINT ( 'NONE',  ( 0.1522836969735572310, -0.4941010236220472751, 6.050992370341708321E-17 ) ) ;
#11615 = LINE ( 'NONE', #22777, #3846 ) ;
#11616 = DIRECTION ( 'NONE',  ( 1.000000000000000000, 0.000000000000000000, 0.000000000000000000 ) ) ;
#11617 = LINE ( 'NONE', #756, #24875 ) ;
#11618 = CARTESIAN_POINT ( 'NONE',  ( 0.3223547283257516272, 0.3832433309296771617, 0.2574803149606298969 ) ) ;
#11619 = AXIS2_PLACEMENT_3D ( 'NONE', #2132, #19222, #4658 ) ;
#11620 = CARTESIAN_POINT ( 'NONE',  ( -1.692913385826771533, 0.07874015748031491790, -0.1181102362204721062 ) ) ;
#11621 = VECTOR ( 'NONE', #22138, 39.37007874015748143 ) ;
#11622 = PRODUCT_DEFINITION_SHAPE ( 'NONE', 'NONE',  #27901 ) ;
#11623 = ORIENTED_EDGE ( 'NONE', *, *, #3387, .T. ) ;
#11624 = CARTESIAN_POINT ( 'NONE',  ( 0.2816963220975960414, 0.2161875334158293027, 1.953740157480315043 ) ) ;
#11625 = ORIENTED_EDGE ( 'NONE', *, *, #7331, .T. ) ;
#11626 = EDGE_CURVE ( 'NONE', #858, #13928, #15919, .T. ) ;
#11627 = CARTESIAN_POINT ( 'NONE',  ( -0.2991932138496239402, -0.3411003281196705594, -1.934055118110236338 ) ) ;
#11628 = CARTESIAN_POINT ( 'NONE',  ( 0.4216927985374664400, -0.2427835582314127327, 0.1827409795180658381 ) ) ;
#11629 = PRESENTATION_LAYER_ASSIGNMENT (  '', '', ( #15273 ) ) ;
#11630 = CYLINDRICAL_SURFACE ( 'NONE', #10666, 0.1308464566929133932 ) ;
#11631 = DIRECTION ( 'NONE',  ( 0.000000000000000000, 0.000000000000000000, -1.000000000000000000 ) ) ;
#11632 = CARTESIAN_POINT ( 'NONE',  ( 0.000000000000000000, 0.000000000000000000, 0.01181102362204724393 ) ) ;
#11633 = DIRECTION ( 'NONE',  ( -1.000000000000000000, 0.000000000000000000, 0.000000000000000000 ) ) ;
#11634 = EDGE_LOOP ( 'NONE', ( #7052, #8787, #14488, #27392 ) ) ;
#11635 = LINE ( 'NONE', #17585, #25772 ) ;
#11636 = EDGE_CURVE ( 'NONE', #27798, #478, #16796, .T. ) ;
#11637 = CARTESIAN_POINT ( 'NONE',  ( 0.000000000000000000, 0.000000000000000000, 0.000000000000000000 ) ) ;
#11638 = DIRECTION ( 'NONE',  ( 1.000000000000000000, 0.000000000000000000, 0.000000000000000000 ) ) ;
#11639 = CARTESIAN_POINT ( 'NONE',  ( -0.3765118517642104257, 0.02464264302297881210, -3.100567304031763172 ) ) ;
#11640 = CARTESIAN_POINT ( 'NONE',  ( -0.2315507648392299000, -0.4792806379917101678, 0.1322834645669291320 ) ) ;
#11641 = CARTESIAN_POINT ( 'NONE',  ( -0.0006620872580285327904, 0.5229309616564024044, 0.1392975274218142823 ) ) ;
#11642 = CONICAL_SURFACE ( 'NONE', #8057, 0.1106489370078740098, 0.08726646250000029414 ) ;
#11643 = VERTEX_POINT ( 'NONE', #21863 ) ;
#11644 = CARTESIAN_POINT ( 'NONE',  ( -0.1432577568504646015, 0.4218945342797250642, -1.934055118110236338 ) ) ;
#11645 = CIRCLE ( 'NONE', #2180, 0.3294268239956709143 ) ;
#11646 = VECTOR ( 'NONE', #6555, 39.37007874015748143 ) ;
#11647 = SHAPE_DEFINITION_REPRESENTATION ( #21323, #12434 ) ;
#11648 = CARTESIAN_POINT ( 'NONE',  ( -0.7432982829791772161, 0.2032415433700952845, -0.2614846436432287091 ) ) ;
#11649 = EDGE_LOOP ( 'NONE', ( #1319, #15798 ) ) ;
#11650 = ORIENTED_EDGE ( 'NONE', *, *, #4311, .F. ) ;
#11651 = AXIS2_PLACEMENT_3D ( 'NONE', #14438, #18784, #23191 ) ;
#11652 = CARTESIAN_POINT ( 'NONE',  ( -0.3681444341728476455, -1.081405805935157449, -0.3462526684107952724 ) ) ;
#11653 = DIRECTION ( 'NONE',  ( 0.000000000000000000, 0.000000000000000000, -1.000000000000000000 ) ) ;
#11654 = CARTESIAN_POINT ( 'NONE',  ( 0.1327036767659691974, 0.4954415918531168139, 1.747047244094488194 ) ) ;
#11655 = ORIENTED_EDGE ( 'NONE', *, *, #14788, .T. ) ;
#11657 = CARTESIAN_POINT ( 'NONE',  ( 0.3726024258163779246, -0.02438677169350792623, -3.115157480314960647 ) ) ;
#11656 = DIRECTION ( 'NONE',  ( 0.000000000000000000, 0.000000000000000000, 1.000000000000000000 ) ) ;
#11658 = EDGE_LOOP ( 'NONE', ( #22526, #10149, #22165, #12741, #21580 ) ) ;
#11659 = DIRECTION ( 'NONE',  ( 0.000000000000000000, -1.000000000000000000, 0.000000000000000000 ) ) ;
#11660 = LINE ( 'NONE', #21855, #4176 ) ;
#11661 = AXIS2_PLACEMENT_3D ( 'NONE', #18004, #26371, #671 ) ;
#11662 = ORIENTED_EDGE ( 'NONE', *, *, #13330, .F. ) ;
#11663 = VERTEX_POINT ( 'NONE', #11120 ) ;
#11664 = CARTESIAN_POINT ( 'NONE',  ( -0.3609634007533684685, -0.7054839598378710441, -0.6417682067245982225 ) ) ;
#11665 = CIRCLE ( 'NONE', #22502, 0.4692913385826771866 ) ;
#11666 = ORIENTED_EDGE ( 'NONE', *, *, #15433, .T. ) ;
#11667 = B_SPLINE_CURVE_WITH_KNOTS ( 'NONE', 3,
 ( #4740, #4484, #21988, #13362, #23843, #13224, #10836, #143, #6879, #17605 ),
 .UNSPECIFIED., .F., .F.,
 ( 4, 2, 2, 2, 4 ),
 ( 0.000000000000000000, 0.2500000000000000000, 0.5000000000000000000, 0.7500000000000000000, 1.000000000000000000 ),
 .UNSPECIFIED. ) ;
#11668 = ORIENTED_EDGE ( 'NONE', *, *, #8644, .F. ) ;
#11669 = CARTESIAN_POINT ( 'NONE',  ( 0.4986013261500205074, 6.106105181202481056E-17, -0.07578740157480315376 ) ) ;
#11670 = ADVANCED_FACE ( 'NONE', ( #17616 ), #5597, .F. ) ;
#11671 = CARTESIAN_POINT ( 'NONE',  ( -0.1786951194748074845, 1.156667798187631879, -0.4648257047102559159 ) ) ;
#11672 = DIRECTION ( 'NONE',  ( 0.000000000000000000, 0.000000000000000000, 1.000000000000000000 ) ) ;
#11673 = AXIS2_PLACEMENT_3D ( 'NONE', #27494, #1912, #14660 ) ;
#11674 = CARTESIAN_POINT ( 'NONE',  ( 0.09842519685039360922, 0.1968503937007873850, -3.272637795275590733 ) ) ;
#11675 = CARTESIAN_POINT ( 'NONE',  ( 0.5620070256527415209, 0.9643919186718870051, -0.1975661767702522054 ) ) ;
#11676 = DIRECTION ( 'NONE',  ( 0.000000000000000000, 1.000000000000000000, 0.000000000000000000 ) ) ;
#11677 = ( BOUNDED_CURVE ( )  B_SPLINE_CURVE ( 2, ( #6430, #17575, #9083 ),
 .UNSPECIFIED., .F., .F. ) 
 B_SPLINE_CURVE_WITH_KNOTS ( ( 3, 3 ),
 ( 0.000000000000000000, 0.5842180690389578990 ),
 .UNSPECIFIED. ) 
 CURVE ( )  GEOMETRIC_REPRESENTATION_ITEM ( )  RATIONAL_B_SPLINE_CURVE ( ( 1.000000000000000000, 1.154700538379245911, 1.000000000000000000 ) ) 
 REPRESENTATION_ITEM ( '' )  ) ;
#11678 = DIRECTION ( 'NONE',  ( 0.000000000000000000, 0.000000000000000000, -1.000000000000000000 ) ) ;
#11679 = FACE_OUTER_BOUND ( 'NONE', #18129, .T. ) ;
#11680 = CARTESIAN_POINT ( 'NONE',  ( 0.6478824768887737617, 0.1135474080050588724, 0.1461456498333656429 ) ) ;
#11681 = CARTESIAN_POINT ( 'NONE',  ( -0.2817310484609166221, 0.2161381151963042424, 1.953740157480315043 ) ) ;
#11682 = CARTESIAN_POINT ( 'NONE',  ( -0.6993003464527065560, -0.1604063846361034051, 0.1601585119460832707 ) ) ;
#11683 = CARTESIAN_POINT ( 'NONE',  ( 0.1517511419331057931, 0.1998583234825911659, -0.4490951218747354923 ) ) ;
#11684 = CIRCLE ( 'NONE', #24770, 0.6299212598425196763 ) ;
#11685 = SPHERICAL_SURFACE ( 'NONE', #15729, 0.07677362204724409722 ) ;
#11686 = VECTOR ( 'NONE', #3261, 39.37007874015748143 ) ;
#11687 = DIRECTION ( 'NONE',  ( -0.9848077530122077983, 0.1736481776669313304, 0.000000000000000000 ) ) ;
#11688 = CARTESIAN_POINT ( 'NONE',  ( -0.4612490782034870396, -0.2663596103035605345, 1.747047244094488194 ) ) ;
#11689 = CARTESIAN_POINT ( 'NONE',  ( -0.1649135259617042215, 0.4856708409200647392, 1.766732283464566899 ) ) ;
#11690 = EDGE_CURVE ( 'NONE', #18223, #23920, #3738, .T. ) ;
#11691 = DIRECTION ( 'NONE',  ( -3.508907999999997507E-18, 0.4999999999999998890, -0.8660254037844388186 ) ) ;
#11692 = VERTEX_POINT ( 'NONE', #26780 ) ;
#11693 = CARTESIAN_POINT ( 'NONE',  ( 0.2952755905264887182, 0.000000000000000000, -3.110236220451535694 ) ) ;
#11694 = ( LENGTH_UNIT ( ) NAMED_UNIT ( * ) SI_UNIT ( $, .METRE. ) ) ;
#11695 = CARTESIAN_POINT ( 'NONE',  ( -0.2341075107471362049, -0.2669897767696617352, 1.953740157480315043 ) ) ;
#11696 = ORIENTED_EDGE ( 'NONE', *, *, #20438, .T. ) ;
#11697 = CARTESIAN_POINT ( 'NONE',  ( 0.1506723201675407575, 0.000000000000000000, 0.000000000000000000 ) ) ;
#11698 = ORIENTED_EDGE ( 'NONE', *, *, #1223, .F. ) ;
#11699 = CARTESIAN_POINT ( 'NONE',  ( 0.2466292688015208900, -0.4270824798167630054, -1.569881889763779625 ) ) ;
#11700 = EDGE_CURVE ( 'NONE', #13428, #20556, #13788, .T. ) ;
#11701 = VERTEX_POINT ( 'NONE', #2894 ) ;
#11702 = CARTESIAN_POINT ( 'NONE',  ( -0.03607471876262562799, -0.5511811023622048555, 0.9399606299212598381 ) ) ;
#11703 = ORIENTED_EDGE ( 'NONE', *, *, #7366, .F. ) ;
#11704 = CARTESIAN_POINT ( 'NONE',  ( 0.4167985568850881561, 0.07349283109919291235, 0.1377952755905511861 ) ) ;
#11705 = AXIS2_PLACEMENT_3D ( 'NONE', #18024, #9861, #3061 ) ;
#11706 = LINE ( 'NONE', #5402, #2001 ) ;
#11707 = DIRECTION ( 'NONE',  ( -0.000000000000000000, -1.000000000000000000, -0.000000000000000000 ) ) ;
#11708 = B_SPLINE_CURVE_WITH_KNOTS ( 'NONE', 3,
 ( #14905, #27746, #25616, #1740, #4009, #12621, #6141, #21240, #10202, #18820, #22941, #27457, #14773, #3862, #10351, #1881, #8390, #10628 ),
 .UNSPECIFIED., .F., .F.,
 ( 4, 2, 2, 2, 2, 2, 2, 2, 4 ),
 ( 0.000000000000000000, 0.2275410946285671421, 0.3413116419428502413, 0.4550821892571332850, 0.5688527365714163286, 0.6826232838856994833, 0.7395085575428416158, 0.7963938311999838593, 0.9101643785142677912 ),
 .UNSPECIFIED. ) ;
#11709 = CARTESIAN_POINT ( 'NONE',  ( 0.4932821129636645874, 0.08637579872942321990, 0.2574803149606298969 ) ) ;
#11710 = CARTESIAN_POINT ( 'NONE',  ( 2.434829265934773153E-16, 0.07874015748031495954, -1.988188976307287970 ) ) ;
#11711 = EDGE_LOOP ( 'NONE', ( #12417, #3603, #20959, #12900 ) ) ;
#11713 = CIRCLE ( 'NONE', #22544, 0.1181102362204720091 ) ;
#11712 = CARTESIAN_POINT ( 'NONE',  ( 0.000000000000000000, 0.000000000000000000, 0.1771653543307086520 ) ) ;
#11714 = CARTESIAN_POINT ( 'NONE',  ( -0.4084310843265718804, 0.3265597623311254916, 0.3331434174597265874 ) ) ;
#11715 = CARTESIAN_POINT ( 'NONE',  ( -0.4246272423000664875, 0.5071139714518992925, 0.1616495878844767808 ) ) ;
#11716 = CARTESIAN_POINT ( 'NONE',  ( 0.08676778863011140597, -0.3239425792934415571, 1.953740157480315043 ) ) ;
#11717 = B_SPLINE_CURVE_WITH_KNOTS ( 'NONE', 3,
 ( #12921, #17174, #2052, #8415, #27352, #4181, #12789, #25788, #8555, #8282 ),
 .UNSPECIFIED., .F., .F.,
 ( 4, 2, 2, 2, 4 ),
 ( 0.000000000000000000, 0.2500000000000000000, 0.5000000000000000000, 0.7500000000000000000, 1.000000000000000000 ),
 .UNSPECIFIED. ) ;
#11718 = DIRECTION ( 'NONE',  ( -1.000000000000000000, 0.000000000000000000, 0.000000000000000000 ) ) ;
#11719 = CARTESIAN_POINT ( 'NONE',  ( -0.1180276236025431524, -0.3257325899126714552, 0.1377952755905512139 ) ) ;
#11720 = DIRECTION ( 'NONE',  ( 0.000000000000000000, 0.000000000000000000, 1.000000000000000000 ) ) ;
#11721 = DIRECTION ( 'NONE',  ( 0.000000000000000000, 0.000000000000000000, -1.000000000000000000 ) ) ;
#11722 = CARTESIAN_POINT ( 'NONE',  ( 0.2228021814283700774, -0.4641672719447021422, 0.3251195115356099175 ) ) ;
#11723 = CARTESIAN_POINT ( 'NONE',  ( 0.1516263115863346334, 0.2937912646890007973, 0.3972688187320929099 ) ) ;
#11724 = DIRECTION ( 'NONE',  ( -0.9848077530122082424, -0.1736481776669300259, 0.000000000000000000 ) ) ;
#11725 = CIRCLE ( 'NONE', #27063, 0.1751968503937007815 ) ;
#11726 = EDGE_CURVE ( 'NONE', #20809, #1867, #26298, .T. ) ;
#11727 = CARTESIAN_POINT ( 'NONE',  ( -0.4986013261500205074, 0.000000000000000000, -0.07578740157480315376 ) ) ;
#11728 = CIRCLE ( 'NONE', #6347, 0.7500000000000001110 ) ;
#11729 = EDGE_CURVE ( 'NONE', #19036, #762, #3985, .T. ) ;
#11730 = EDGE_CURVE ( 'NONE', #3239, #25537, #5561, .T. ) ;
#11731 = ORIENTED_EDGE ( 'NONE', *, *, #14957, .F. ) ;
#11732 = CARTESIAN_POINT ( 'NONE',  ( 0.000000000000000000, 0.000000000000000000, -1.092739370078740131E-17 ) ) ;
#11733 = EDGE_CURVE ( 'NONE', #3772, #9494, #20328, .T. ) ;
#11734 = DIRECTION ( 'NONE',  ( -1.000000000000000000, 0.000000000000000000, 0.000000000000000000 ) ) ;
#11735 = VERTEX_POINT ( 'NONE', #26635 ) ;
#11736 = CARTESIAN_POINT ( 'NONE',  ( -0.01030706208231915028, 0.1968503937007873850, -3.626968503937007871 ) ) ;
#11737 = ORIENTED_EDGE ( 'NONE', *, *, #15737, .T. ) ;
#11738 = FACE_OUTER_BOUND ( 'NONE', #8717, .T. ) ;
#11739 = ORIENTED_EDGE ( 'NONE', *, *, #5914, .F. ) ;
#11740 = DIRECTION ( 'NONE',  ( 1.000000000000000000, 0.000000000000000000, 0.000000000000000000 ) ) ;
#11741 = CARTESIAN_POINT ( 'NONE',  ( 0.7873253891977465280, 0.2508138056050463471, -0.2773433314823283702 ) ) ;
#11742 = B_SPLINE_CURVE_WITH_KNOTS ( 'NONE', 3,
 ( #20004, #525, #26628, #26091, #24507, #6752, #17475, #4607 ),
 .UNSPECIFIED., .F., .F.,
 ( 4, 2, 2, 4 ),
 ( 0.000000000000000000, 0.2500000000000002776, 0.5000000000000005551, 1.000000000000000000 ),
 .UNSPECIFIED. ) ;
#11743 = AXIS2_PLACEMENT_3D ( 'NONE', #11124, #8454, #13240 ) ;
#11744 = CARTESIAN_POINT ( 'NONE',  ( 0.5511811023622047445, 0.000000000000000000, -1.550196850393700920 ) ) ;
#11745 = ORIENTED_EDGE ( 'NONE', *, *, #14857, .F. ) ;
#11746 = ORIENTED_EDGE ( 'NONE', *, *, #21955, .F. ) ;
#11747 = CARTESIAN_POINT ( 'NONE',  ( 0.1522836969735573143, -0.4909267390297480382, 0.05591742528025181458 ) ) ;
#11748 = CARTESIAN_POINT ( 'NONE',  ( 0.4889536969034952718, -0.06441834428466330920, -1.550196850393700920 ) ) ;
#11749 = CARTESIAN_POINT ( 'NONE',  ( -0.5177165354330708347, -0.4724409448818898127, 0.8182917201112794858 ) ) ;
#11750 = CARTESIAN_POINT ( 'NONE',  ( -0.5230301363771269196, -0.1775991818008745282, 0.9202755905511811330 ) ) ;
#11751 = LINE ( 'NONE', #22633, #12095 ) ;
#11752 = CARTESIAN_POINT ( 'NONE',  ( 0.1285103288269283661, -0.3545966721392122545, 0.07637795275590551769 ) ) ;
#11753 = DIRECTION ( 'NONE',  ( -0.000000000000000000, -0.000000000000000000, -1.000000000000000000 ) ) ;
#11754 = ADVANCED_FACE ( 'NONE', ( #18426 ), #13112, .T. ) ;
#11755 = CARTESIAN_POINT ( 'NONE',  ( 0.000000000000000000, 0.000000000000000000, -4.330708661417323135 ) ) ;
#11756 = ORIENTED_EDGE ( 'NONE', *, *, #24323, .T. ) ;
#11757 = CARTESIAN_POINT ( 'NONE',  ( -0.6299212598425196763, 0.9448818897637796255, -9.561468503937007847E-18 ) ) ;
#11758 = DIRECTION ( 'NONE',  ( 0.000000000000000000, 0.000000000000000000, 1.000000000000000000 ) ) ;
#11759 = DIRECTION ( 'NONE',  ( 0.000000000000000000, 0.000000000000000000, 1.000000000000000000 ) ) ;
#11760 = EDGE_CURVE ( 'NONE', #8441, #2885, #8163, .T. ) ;
#11761 = DIRECTION ( 'NONE',  ( -0.9790454724845842893, 0.1018208755700880375, 0.1763589297585410332 ) ) ;
#11762 = ORIENTED_EDGE ( 'NONE', *, *, #2969, .T. ) ;
#11763 = AXIS2_PLACEMENT_3D ( 'NONE', #14522, #3754, #12375 ) ;
#11764 = ( LENGTH_UNIT ( ) NAMED_UNIT ( * ) SI_UNIT ( $, .METRE. ) ) ;
#11765 = CARTESIAN_POINT ( 'NONE',  ( -7.608238775805210269E-17, -0.6212598425196850238, 0.04842519685039370358 ) ) ;
#11766 = CARTESIAN_POINT ( 'NONE',  ( -0.6299212598425196763, -0.4724409448818898127, -0.8182917201112815953 ) ) ;
#11767 = ORIENTED_EDGE ( 'NONE', *, *, #1109, .F. ) ;
#11768 = CARTESIAN_POINT ( 'NONE',  ( -0.3543321272855304849, 0.02325127328527686055, 1.953740157480315709 ) ) ;
#11769 = ORIENTED_EDGE ( 'NONE', *, *, #13508, .T. ) ;
#11770 = EDGE_LOOP ( 'NONE', ( #1007, #27039, #18557, #17960 ) ) ;
#11771 = AXIS2_PLACEMENT_3D ( 'NONE', #23551, #20991, #3753 ) ;
#11772 = CARTESIAN_POINT ( 'NONE',  ( 0.3929158813954871654, 0.2268989272875732710, -1.934055118110236338 ) ) ;
#11773 = ( GEOMETRIC_REPRESENTATION_CONTEXT ( 3 ) GLOBAL_UNCERTAINTY_ASSIGNED_CONTEXT ( ( #14129 ) ) GLOBAL_UNIT_ASSIGNED_CONTEXT ( ( #14822, #4064, #8436 ) ) REPRESENTATION_CONTEXT ( 'NONE', 'WORKASPACE' ) ) ;
#11774 = LINE ( 'NONE', #20392, #3551 ) ;
#11775 = CARTESIAN_POINT ( 'NONE',  ( -0.1718374205099799101, -0.4703827404237102550, 0.09685039370078740717 ) ) ;
#11776 = CARTESIAN_POINT ( 'NONE',  ( 0.1490609433576163545, -0.2393035190829114200, 0.4144858534816307505 ) ) ;
#11777 = CARTESIAN_POINT ( 'NONE',  ( -0.01968503937007873988, -0.6102362204724409711, 0.000000000000000000 ) ) ;
#11778 = CARTESIAN_POINT ( 'NONE',  ( 1.877524803149606209E-16, 0.3149606299212598381, 0.000000000000000000 ) ) ;
#11779 = VERTEX_POINT ( 'NONE', #7291 ) ;
#11780 = EDGE_CURVE ( 'NONE', #26494, #15892, #12648, .T. ) ;
#11781 = CARTESIAN_POINT ( 'NONE',  ( -0.4417544603400644920, -0.05811278586497442555, -1.934055118110237004 ) ) ;
#11782 = ORIENTED_EDGE ( 'NONE', *, *, #9257, .F. ) ;
#11783 = CARTESIAN_POINT ( 'NONE',  ( 0.5949363243629232079, -0.1357903337134992172, 0.3661437007874016047 ) ) ;
#11784 = APPLICATION_CONTEXT ( 'automotive_design' ) ;
#11785 = EDGE_LOOP ( 'NONE', ( #11109, #19027 ) ) ;
#11786 = CARTESIAN_POINT ( 'NONE',  ( -0.1970259548081969847, -0.3996230174612658281, -1.934055118110236338 ) ) ;
#11787 = AXIS2_PLACEMENT_3D ( 'NONE', #27186, #10353, #18540 ) ;
#11788 = CARTESIAN_POINT ( 'NONE',  ( -0.3979194638820449104, -0.2297883689023288989, -1.928289503579160513 ) ) ;
#11789 = APPLICATION_PROTOCOL_DEFINITION ( 'draft international standard', 'automotive_design', 1998, #11784 ) ;
#11790 = CIRCLE ( 'NONE', #4128, 0.1476377952755905387 ) ;
#11791 = EDGE_CURVE ( 'NONE', #25, #5266, #8991, .T. ) ;
#11792 = ORIENTED_EDGE ( 'NONE', *, *, #25585, .T. ) ;
#11793 = VERTEX_POINT ( 'NONE', #5162 ) ;
#11794 = CARTESIAN_POINT ( 'NONE',  ( 0.07874015748031495954, 0.1968503937007873850, -3.364501312335955063 ) ) ;
#11795 = DIRECTION ( 'NONE',  ( 0.000000000000000000, 0.000000000000000000, 1.000000000000000000 ) ) ;
#11796 = CARTESIAN_POINT ( 'NONE',  ( 0.4954415918530851726, -0.1327036767659643957, 1.766732283464566899 ) ) ;
#11797 = ADVANCED_FACE ( 'NONE', ( #11524 ), #4090, .T. ) ;
#11798 = CARTESIAN_POINT ( 'NONE',  ( 0.000000000000000000, 0.000000000000000000, -0.2755905511811023723 ) ) ;
#11799 = CARTESIAN_POINT ( 'NONE',  ( 0.2993674444872273521, 0.2296683860596781812, -3.100567304031764060 ) ) ;
#11800 = CARTESIAN_POINT ( 'NONE',  ( -0.6029884523518272976, 1.118955382540533838, -0.03814816047821503742 ) ) ;
#11801 = DIRECTION ( 'NONE',  ( 1.000000000000000000, 7.017815000000000124E-18, 0.000000000000000000 ) ) ;
#11802 = ADVANCED_FACE ( 'NONE', ( #24797 ), #20145, .T. ) ;
#11803 = ORIENTED_EDGE ( 'NONE', *, *, #18215, .F. ) ;
#11804 = EDGE_LOOP ( 'NONE', ( #25172, #9845, #6829, #7360, #18069, #2227 ) ) ;
#11805 = AXIS2_PLACEMENT_3D ( 'NONE', #25052, #6145, #14332 ) ;
#11806 = EDGE_LOOP ( 'NONE', ( #3946, #18936, #2135, #18787 ) ) ;
#11807 = FACE_OUTER_BOUND ( 'NONE', #6003, .T. ) ;
#11808 = CARTESIAN_POINT ( 'NONE',  ( -0.07217847769028858107, 0.04546065111729338110, 0.000000000000000000 ) ) ;
#11809 = ORIENTED_EDGE ( 'NONE', *, *, #6996, .T. ) ;
#11810 = CARTESIAN_POINT ( 'NONE',  ( -0.1970259548081969847, -0.3996230174612658281, -1.934055118110236338 ) ) ;
#11811 = VERTEX_POINT ( 'NONE', #9533 ) ;
#11812 = DIRECTION ( 'NONE',  ( 0.000000000000000000, -1.224646707287115868E-16, -1.000000000000000000 ) ) ;
#11813 = PLANE ( 'NONE',  #17162 ) ;
#11814 = EDGE_CURVE ( 'NONE', #14891, #23446, #16055, .T. ) ;
#11815 = AXIS2_PLACEMENT_3D ( 'NONE', #19415, #8943, #13181 ) ;
#11816 = CARTESIAN_POINT ( 'NONE',  ( -0.3102476824511312681, 0.1791601451669032896, -3.115157480314960647 ) ) ;
#11817 = DIRECTION ( 'NONE',  ( 0.000000000000000000, 0.000000000000000000, -1.000000000000000000 ) ) ;
#11818 = CARTESIAN_POINT ( 'NONE',  ( -0.2056553984168022209, 0.2676050456844303316, 1.973425196850394414 ) ) ;
#11819 = FACE_OUTER_BOUND ( 'NONE', #2407, .T. ) ;
#11820 = DIRECTION ( 'NONE',  ( 0.000000000000000000, -1.000000000000000000, 0.000000000000000000 ) ) ;
#11821 = CARTESIAN_POINT ( 'NONE',  ( 0.5187889641967551313, -0.1190953285357214675, 0.3401574803149606252 ) ) ;
#11822 = CARTESIAN_POINT ( 'NONE',  ( 0.1141709026133613525, -0.3362336590883617249, 1.953740157480315043 ) ) ;
#11823 = ORIENTED_EDGE ( 'NONE', *, *, #6894, .F. ) ;
#11824 = CARTESIAN_POINT ( 'NONE',  ( -0.6864238947242438105, -0.1574599019772051633, 0.3281099440175202497 ) ) ;
#11825 = AXIS2_PLACEMENT_3D ( 'NONE', #12271, #13987, #10147 ) ;
#11826 = CARTESIAN_POINT ( 'NONE',  ( 0.3214446924536846772, 0.3840069416942866742, 0.09685039370078740717 ) ) ;
#11827 = CARTESIAN_POINT ( 'NONE',  ( 0.3937007873768824662, 0.000000000000000000, -4.330708661417323135 ) ) ;
#11828 = FACE_OUTER_BOUND ( 'NONE', #14862, .T. ) ;
#11829 = CARTESIAN_POINT ( 'NONE',  ( -0.4225965726692976765, -0.3242071728275119913, 1.747047244094488194 ) ) ;
#11830 = DIRECTION ( 'NONE',  ( 0.000000000000000000, 1.000000000000000000, 0.000000000000000000 ) ) ;
#11831 = EDGE_CURVE ( 'NONE', #3892, #27393, #20776, .T. ) ;
#11832 = CARTESIAN_POINT ( 'NONE',  ( 0.03349795313264414959, -0.5118110236220471121, 1.766732283464566899 ) ) ;
#11833 = AXIS2_PLACEMENT_3D ( 'NONE', #20720, #5761, #20859 ) ;
#11834 = EDGE_CURVE ( 'NONE', #496, #2802, #8677, .T. ) ;
#11835 = ORIENTED_EDGE ( 'NONE', *, *, #5501, .T. ) ;
#11836 = DIRECTION ( 'NONE',  ( 0.000000000000000000, 1.000000000000000000, -1.224646799147353207E-16 ) ) ;
#11837 = ORIENTED_EDGE ( 'NONE', *, *, #25230, .F. ) ;
#11838 = FACE_OUTER_BOUND ( 'NONE', #21591, .T. ) ;
#11839 = ( LENGTH_UNIT ( ) NAMED_UNIT ( * ) SI_UNIT ( $, .METRE. ) ) ;
#11840 = DIRECTION ( 'NONE',  ( -0.9396926207859082059, 0.3420201433256689905, 0.000000000000000000 ) ) ;
#11841 = PLANE ( 'NONE',  #11238 ) ;
#11842 = ORIENTED_EDGE ( 'NONE', *, *, #16550, .F. ) ;
#11843 = CARTESIAN_POINT ( 'NONE',  ( -0.2180862235769562008, -0.4423390553432419714, -1.569881889763779625 ) ) ;
#11844 = CARTESIAN_POINT ( 'NONE',  ( 0.4338922498494567348, -0.2500511477696476526, 0.09684874903502814492 ) ) ;
#11845 = VERTEX_POINT ( 'NONE', #10524 ) ;
#11846 = ORIENTED_EDGE ( 'NONE', *, *, #7388, .T. ) ;
#11847 = CIRCLE ( 'NONE', #24030, 0.1771653543307086798 ) ;
#11848 = AXIS2_PLACEMENT_3D ( 'NONE', #8932, #6551, #23927 ) ;
#11849 = DIRECTION ( 'NONE',  ( 1.000000000000000000, 0.000000000000000000, 0.000000000000000000 ) ) ;
#11850 = DIRECTION ( 'NONE',  ( 0.000000000000000000, 0.000000000000000000, -1.000000000000000000 ) ) ;
#11851 = CARTESIAN_POINT ( 'NONE',  ( 4.821444091131312140E-17, 0.9055118110236221041, 0.3937007874015748254 ) ) ;
#11852 = DIRECTION ( 'NONE',  ( 0.000000000000000000, 1.000000000000000000, 0.000000000000000000 ) ) ;
#11853 = EDGE_CURVE ( 'NONE', #11391, #15542, #15399, .T. ) ;
#11854 = CIRCLE ( 'NONE', #15028, 0.09842519685039370636 ) ;
#11855 = CARTESIAN_POINT ( 'NONE',  ( 0.4165721057576322606, 0.3313508221749649763, 0.3401574803149606252 ) ) ;
#11856 = CARTESIAN_POINT ( 'NONE',  ( -0.3007905576423956506, 0.1482986320106521871, 1.953740157480315043 ) ) ;
#11857 = UNCERTAINTY_MEASURE_WITH_UNIT (LENGTH_MEASURE( 1.000000000000000082E-05 ), #3369, 'distance_accuracy_value', 'NONE') ;
#11858 = ORIENTED_EDGE ( 'NONE', *, *, #20245, .T. ) ;
#11859 = DIRECTION ( 'NONE',  ( 0.000000000000000000, 0.000000000000000000, 1.000000000000000000 ) ) ;
#11860 = PLANE ( 'NONE',  #7856 ) ;
#11861 = DIRECTION ( 'NONE',  ( 0.000000000000000000, 0.000000000000000000, 1.000000000000000000 ) ) ;
#11862 = CARTESIAN_POINT ( 'NONE',  ( -0.4984899526255159863, -0.1339654526248284516, 1.766732283464567121 ) ) ;
#11863 = DIRECTION ( 'NONE',  ( 1.000000000000000000, 0.000000000000000000, 0.000000000000000000 ) ) ;
#11864 = PRODUCT_DEFINITION_SHAPE ( 'NONE', 'NONE',  #27920 ) ;
#11865 = CARTESIAN_POINT ( 'NONE',  ( -0.3777066424200924422, 0.3020248451651783017, 0.2008762815972411353 ) ) ;
#11866 = VECTOR ( 'NONE', #19533, 39.37007874015748143 ) ;
#11867 = DIRECTION ( 'NONE',  ( 0.000000000000000000, 0.000000000000000000, 1.000000000000000000 ) ) ;
#11868 = AXIS2_PLACEMENT_3D ( 'NONE', #9762, #18220, #2967 ) ;
#11869 = CARTESIAN_POINT ( 'NONE',  ( 0.5085287184740714395, 0.06690297524259165851, -1.550196850393700920 ) ) ;
#11870 = ORIENTED_EDGE ( 'NONE', *, *, #14644, .T. ) ;
#11871 = SHAPE_REPRESENTATION_RELATIONSHIP ( 'NONE' , 'NONE' ,  #4612, #3606 ) ;
#11872 = ORIENTED_EDGE ( 'NONE', *, *, #10320, .T. ) ;
#11873 = CIRCLE ( 'NONE', #5085, 1.131889763779527547 ) ;
#11874 = CARTESIAN_POINT ( 'NONE',  ( -0.3121994997578409481, -0.4069448477569437284, -1.550196850393700920 ) ) ;
#11875 = DIRECTION ( 'NONE',  ( 0.000000000000000000, 1.000000000000000000, 0.000000000000000000 ) ) ;
#11876 = AXIS2_PLACEMENT_3D ( 'NONE', #13113, #19626, #2235 ) ;
#11877 = CARTESIAN_POINT ( 'NONE',  ( -0.02061007003135920460, 0.1968503937007873850, -3.624919108234672560 ) ) ;
#11878 = VERTEX_POINT ( 'NONE', #16751 ) ;
#11879 = DIRECTION ( 'NONE',  ( 0.000000000000000000, 1.000000000000000000, 0.000000000000000000 ) ) ;
#11880 = ORIENTED_EDGE ( 'NONE', *, *, #7592, .F. ) ;
#11881 = CARTESIAN_POINT ( 'NONE',  ( 0.5309636003393858328, 0.7559193067387677267, -0.4362061884873984496 ) ) ;
#11882 = EDGE_CURVE ( 'NONE', #19638, #27384, #26882, .T. ) ;
#11883 = CIRCLE ( 'NONE', #4664, 0.3771653543307086909 ) ;
#11884 = ADVANCED_FACE ( 'NONE', ( #27638 ), #16901, .T. ) ;
#11885 = CONICAL_SURFACE ( 'NONE', #27691, 0.4724409448818898127, 0.7853981625000003852 ) ;
#11886 = CARTESIAN_POINT ( 'NONE',  ( 0.2990496115118929099, -0.6198172806991221195, 0.1322818203437344520 ) ) ;
#11887 = VERTEX_POINT ( 'NONE', #20844 ) ;
#11888 = CARTESIAN_POINT ( 'NONE',  ( -0.3722026523000413478, 0.000000000000000000, -0.05856299212598425896 ) ) ;
#11889 = PRODUCT_DEFINITION ( 'UNKNOWN', '', #7114, #20685 ) ;
#11890 = VERTEX_POINT ( 'NONE', #12228 ) ;
#11891 = CARTESIAN_POINT ( 'NONE',  ( -0.2041304421298332783, 0.2660793235464289364, 1.973425196850393970 ) ) ;
#11892 = CARTESIAN_POINT ( 'NONE',  ( -0.1327036767636080028, -0.4954415918535519658, -1.550196850393700920 ) ) ;
#11893 = EDGE_CURVE ( 'NONE', #15321, #8729, #13544, .T. ) ;
#11894 = CARTESIAN_POINT ( 'NONE',  ( -0.4713455951419531220, -0.1082342125229185797, 0.2715646632656424919 ) ) ;
#11895 = CARTESIAN_POINT ( 'NONE',  ( -0.5511811023622047445, -0.03607471876259067678, 0.9202755905511811330 ) ) ;
#11896 = FACE_OUTER_BOUND ( 'NONE', #14864, .T. ) ;
#11897 = EDGE_CURVE ( 'NONE', #14000, #12475, #3618, .T. ) ;
#11898 = AXIS2_PLACEMENT_3D ( 'NONE', #26686, #20625, #15967 ) ;
#11899 = DIRECTION ( 'NONE',  ( 0.000000000000000000, 0.000000000000000000, -1.000000000000000000 ) ) ;
#11900 = VERTEX_POINT ( 'NONE', #10238 ) ;
#11901 = CARTESIAN_POINT ( 'NONE',  ( 0.000000000000000000, 0.000000000000000000, 0.3401574803149606252 ) ) ;
#11902 = B_SPLINE_CURVE_WITH_KNOTS ( 'NONE', 3,
 ( #17255, #25872, #23900, #26144, #15431, #21911, #1994, #24023, #26274, #19508 ),
 .UNSPECIFIED., .F., .F.,
 ( 4, 2, 2, 2, 4 ),
 ( 0.000000000000000000, 0.2500000000000000000, 0.5000000000000000000, 0.7500000000000000000, 1.000000000000000000 ),
 .UNSPECIFIED. ) ;
#11903 = SURFACE_STYLE_FILL_AREA ( #24891 ) ;
#11904 = VERTEX_POINT ( 'NONE', #18853 ) ;
#11905 = CARTESIAN_POINT ( 'NONE',  ( 0.1819818857492424280, 0.6289820519968024604, 0.07987519446618293606 ) ) ;
#11906 = CARTESIAN_POINT ( 'NONE',  ( -0.2662790972932065348, 0.4613045817965927831, 1.747047244094488638 ) ) ;
#11907 = DIRECTION ( 'NONE',  ( -1.000000000000000000, 0.000000000000000000, 0.000000000000000000 ) ) ;
#11908 = ORIENTED_EDGE ( 'NONE', *, *, #25231, .F. ) ;
#11909 = ORIENTED_EDGE ( 'NONE', *, *, #2419, .T. ) ;
#11911 = CARTESIAN_POINT ( 'NONE',  ( 0.3905379133858267737, 0.5610236220472440971, 0.000000000000000000 ) ) ;
#11912 = CARTESIAN_POINT ( 'NONE',  ( -4.821283464566928349E-18, 0.000000000000000000, -0.3779527559055118058 ) ) ;
#11913 = ORIENTED_EDGE ( 'NONE', *, *, #23131, .T. ) ;
#11914 = CARTESIAN_POINT ( 'NONE',  ( -0.2161875334158534223, 0.2816963220975619575, 1.953740157480314821 ) ) ;
#11915 = ORIENTED_EDGE ( 'NONE', *, *, #3797, .T. ) ;
#11916 = ORIENTED_EDGE ( 'NONE', *, *, #3524, .F. ) ;
#11917 = AXIS2_PLACEMENT_3D ( 'NONE', #4806, #584, #13701 ) ;
#11918 = CARTESIAN_POINT ( 'NONE',  ( 0.2268989272875507057, -0.3929158813954434226, -1.934055118110236338 ) ) ;
#11919 = CARTESIAN_POINT ( 'NONE',  ( 0.3334645669291338987, 0.000000000000000000, -1.052618110236220428 ) ) ;
#11920 = CARTESIAN_POINT ( 'NONE',  ( -0.1603262695921763847, -0.4410554214326614098, 0.1992150590373740204 ) ) ;
#11921 = CARTESIAN_POINT ( 'NONE',  ( 0.1490609433494345937, -0.2474992208661806470, -0.4097540628404507945 ) ) ;
#11922 = CIRCLE ( 'NONE', #13721, 0.5118110236220472231 ) ;
#11923 = DIRECTION ( 'NONE',  ( 0.000000000000000000, 0.000000000000000000, 1.000000000000000000 ) ) ;
#11924 = VERTEX_POINT ( 'NONE', #1494 ) ;
#11925 = CARTESIAN_POINT ( 'NONE',  ( -2.685748425196850164E-17, 0.000000000000000000, -1.934055118110236338 ) ) ;
#11926 = CARTESIAN_POINT ( 'NONE',  ( -0.3070866141732283561, 3.760726391082423050E-17, 0.2755905511811023723 ) ) ;
#11927 = CARTESIAN_POINT ( 'NONE',  ( -0.2315507648392299000, -0.4792806379917101678, 0.1322834645669291320 ) ) ;
#11928 = ORIENTED_EDGE ( 'NONE', *, *, #6645, .F. ) ;
#11929 = CARTESIAN_POINT ( 'NONE',  ( -0.3740848232703753440, -0.04928467685643751067, -3.100567304031760507 ) ) ;
#11930 = CARTESIAN_POINT ( 'NONE',  ( 0.3213085410496531180, -0.1584824234588266545, -3.115157480314961091 ) ) ;
#11931 = EDGE_CURVE ( 'NONE', #14590, #26957, #16261, .T. ) ;
#11932 = CIRCLE ( 'NONE', #14203, 0.2395669291338582696 ) ;
#11933 = ORIENTED_EDGE ( 'NONE', *, *, #18967, .T. ) ;
#11934 = CARTESIAN_POINT ( 'NONE',  ( -0.4527559054764770385, 0.000000000000000000, -1.934055118110236338 ) ) ;
#11935 = EDGE_CURVE ( 'NONE', #3730, #15240, #14662, .T. ) ;
#11936 = CIRCLE ( 'NONE', #18673, 0.8267716535433071723 ) ;
#11937 = VERTEX_POINT ( 'NONE', #23266 ) ;
#11938 = ORIENTED_EDGE ( 'NONE', *, *, #6655, .F. ) ;
#11939 = CIRCLE ( 'NONE', #18699, 0.7874015748031496509 ) ;
#11940 = CARTESIAN_POINT ( 'NONE',  ( 0.09842519685039366473, 0.1968503937007873850, -3.364501312335956396 ) ) ;
#11941 = DIRECTION ( 'NONE',  ( -1.000000000000000000, 0.000000000000000000, 0.000000000000000000 ) ) ;
#11942 = CARTESIAN_POINT ( 'NONE',  ( 0.5144970376936013334, 0.1378076643338890239, 1.747047244094488194 ) ) ;
#11943 = ORIENTED_EDGE ( 'NONE', *, *, #4096, .T. ) ;
#11944 = ORIENTED_EDGE ( 'NONE', *, *, #1539, .T. ) ;
#11945 = ADVANCED_FACE ( 'NONE', ( #12514 ), #21130, .F. ) ;
#11946 = VERTEX_POINT ( 'NONE', #22979 ) ;
#11947 = CARTESIAN_POINT ( 'NONE',  ( 0.02464264302293732445, -0.3765118517642105367, -3.100567304031763172 ) ) ;
#11948 = ORIENTED_EDGE ( 'NONE', *, *, #9231, .F. ) ;
#11949 = DIRECTION ( 'NONE',  ( -1.000000000000000000, 0.000000000000000000, 0.000000000000000000 ) ) ;
#11950 = CARTESIAN_POINT ( 'NONE',  ( 0.04115487667019134682, -0.6180305271469684891, 0.08832868324785138336 ) ) ;
#11951 = VECTOR ( 'NONE', #19962, 39.37007874015748854 ) ;
#11952 = ORIENTED_EDGE ( 'NONE', *, *, #25299, .F. ) ;
#11953 = CARTESIAN_POINT ( 'NONE',  ( -0.4307861782378184512, -0.5235511812839959145, -0.4261998249987570264 ) ) ;
#11954 = DIRECTION ( 'NONE',  ( 1.000000000000000000, 0.000000000000000000, 0.000000000000000000 ) ) ;
#11955 = CARTESIAN_POINT ( 'NONE',  ( 0.3996230174612959707, 0.1970259548082022305, -1.934055118110236338 ) ) ;
#11956 = ORIENTED_EDGE ( 'NONE', *, *, #7820, .T. ) ;
#11957 = EDGE_LOOP ( 'NONE', ( #10463, #5502, #21452, #18584 ) ) ;
#11958 = DIRECTION ( 'NONE',  ( -0.000000000000000000, -0.000000000000000000, 1.000000000000000000 ) ) ;
#11959 = FACE_BOUND ( 'NONE', #8549, .T. ) ;
#11960 = CIRCLE ( 'NONE', #23247, 0.2952755905511810774 ) ;
#11961 = CARTESIAN_POINT ( 'NONE',  ( 0.04679574315772144777, 0.3551931031211610912, -3.115157480314960647 ) ) ;
#11962 = CIRCLE ( 'NONE', #9232, 0.4330708661417322913 ) ;
#11963 = CARTESIAN_POINT ( 'NONE',  ( 0.000000000000000000, 0.000000000000000000, 0.4488188976377953110 ) ) ;
#11964 = CARTESIAN_POINT ( 'NONE',  ( 0.5530354143091553709, 0.9746577485994293299, -0.2092867075132898436 ) ) ;
#11965 = CARTESIAN_POINT ( 'NONE',  ( 0.7874015748031496509, 3.035194737559055338E-06, -1.475314960619023674 ) ) ;
#11966 = EDGE_CURVE ( 'NONE', #1047, #7118, #22486, .T. ) ;
#11967 = CARTESIAN_POINT ( 'NONE',  ( -0.08600259727896246431, 0.2165354330708661457, -3.223068997994991580 ) ) ;
#11968 = CARTESIAN_POINT ( 'NONE',  ( -0.08759279594700329630, -0.3259357382551448246, 1.973425196850394192 ) ) ;
#11969 = CARTESIAN_POINT ( 'NONE',  ( 0.5382469622846756119, -0.3102483656526354716, 0.2574819594177531479 ) ) ;
#11970 = AXIS2_PLACEMENT_3D ( 'NONE', #13819, #11691, #20311 ) ;
#11971 = VERTEX_POINT ( 'NONE', #20660 ) ;
#11972 = CARTESIAN_POINT ( 'NONE',  ( 0.5890517850735842442, -0.1332273157280143838, -0.2362204724409449064 ) ) ;
#11974 = ADVANCED_FACE ( 'NONE', ( #897 ), #18976, .F. ) ;
#11973 = CARTESIAN_POINT ( 'NONE',  ( 0.000000000000000000, 0.000000000000000000, -4.330708661417323135 ) ) ;
#11975 = MANIFOLD_SOLID_BREP ( 'Rear Bearing Cover', #22269 ) ;
#11976 = FACE_BOUND ( 'NONE', #25512, .T. ) ;
#11977 = CARTESIAN_POINT ( 'NONE',  ( 0.2268096725222282783, -0.4600326175560538466, 1.747047244094488194 ) ) ;
#11978 = CARTESIAN_POINT ( 'NONE',  ( -0.4600326175560602304, -0.2268096725222347454, 1.766732283464566899 ) ) ;
#11979 = EDGE_CURVE ( 'NONE', #25145, #7459, #3544, .T. ) ;
#11980 = CIRCLE ( 'NONE', #22337, 0.1771653543307086798 ) ;
#11981 = CARTESIAN_POINT ( 'NONE',  ( 0.1718374205099799101, -0.4703827404237102550, 0.09685039370078740717 ) ) ;
#11982 = VERTEX_POINT ( 'NONE', #7238 ) ;
#11983 = VECTOR ( 'NONE', #11453, 39.37007874015748143 ) ;
#11984 = CARTESIAN_POINT ( 'NONE',  ( 0.000000000000000000, 0.3937007874015748254, 0.01181102362204724393 ) ) ;
#11985 = SHAPE_REPRESENTATION_RELATIONSHIP ( 'NONE' , 'NONE' ,  #3575, #27550 ) ;
#11986 = CYLINDRICAL_SURFACE ( 'NONE', #26879, 0.8267716535433071723 ) ;
#11987 = CARTESIAN_POINT ( 'NONE',  ( 0.3339160553493882300, 0.7867001919223544082, -0.8344257386302499357 ) ) ;
#11988 = CARTESIAN_POINT ( 'NONE',  ( 0.000000000000000000, 0.000000000000000000, -0.4724409448818898127 ) ) ;
#11989 = VERTEX_POINT ( 'NONE', #15854 ) ;
#11990 = VERTEX_POINT ( 'NONE', #22499 ) ;
#11991 = TOROIDAL_SURFACE ( 'NONE', #6160, 0.4232283464566928832, 0.07677165354330708902 ) ;
#11992 = CARTESIAN_POINT ( 'NONE',  ( -0.1275996891957758561, 0.4763861460130329184, -1.569881889763779625 ) ) ;
#11993 = VERTEX_POINT ( 'NONE', #1178 ) ;
#11994 = ORIENTED_EDGE ( 'NONE', *, *, #11440, .F. ) ;
#11995 = AXIS2_PLACEMENT_3D ( 'NONE', #17297, #10514, #4449 ) ;
#11996 = EDGE_CURVE ( 'NONE', #1231, #19596, #15812, .T. ) ;
#11997 = CARTESIAN_POINT ( 'NONE',  ( 0.1490609433494345937, 0.4786070381568061083, -0.009463581267948129386 ) ) ;
#11998 = CARTESIAN_POINT ( 'NONE',  ( 0.3458446900868161200, 4.235375927169277411E-17, -0.2204724409448818867 ) ) ;
#11999 = LINE ( 'NONE', #21032, #24928 ) ;
#12000 = ADVANCED_FACE ( 'NONE', ( #22638, #16151 ), #26583, .T. ) ;
#12001 = VERTEX_POINT ( 'NONE', #27025 ) ;
#12002 = CARTESIAN_POINT ( 'NONE',  ( -0.4092566936335077510, 0.3255244810064202854, 0.3331434174600059750 ) ) ;
#12003 = AXIS2_PLACEMENT_3D ( 'NONE', #20042, #9427, #26392 ) ;
#12004 = CARTESIAN_POINT ( 'NONE',  ( -0.2041304421298503480, 0.2660793235464394280, 1.953740157480315043 ) ) ;
#12005 = DIRECTION ( 'NONE',  ( 1.000000000000000000, 0.000000000000000000, 0.000000000000000000 ) ) ;
#12006 = DIRECTION ( 'NONE',  ( 0.000000000000000000, 1.000000000000000000, 0.000000000000000000 ) ) ;
#12007 = CARTESIAN_POINT ( 'NONE',  ( 0.4067073728345488304, -0.2341441294389854655, 0.07637795275590551769 ) ) ;
#12008 = DIRECTION ( 'NONE',  ( 0.000000000000000000, 0.000000000000000000, 1.000000000000000000 ) ) ;
#12009 = VECTOR ( 'NONE', #23077, 39.37007874015748854 ) ;
#12010 = DIRECTION ( 'NONE',  ( -1.000000000000000000, 0.000000000000000000, 0.000000000000000000 ) ) ;
#12011 = CARTESIAN_POINT ( 'NONE',  ( 0.1601448837025137850, -0.4411213145380133982, 0.1992142434433712694 ) ) ;
#12012 = CARTESIAN_POINT ( 'NONE',  ( -0.3024344094364738722, 0.3935368318888683437, -1.569881889763779625 ) ) ;
#12013 = CARTESIAN_POINT ( 'NONE',  ( 0.000000000000000000, 0.9055118110236221041, 0.000000000000000000 ) ) ;
#12014 = EDGE_CURVE ( 'NONE', #13235, #8311, #1822, .T. ) ;
#12015 = ORIENTED_EDGE ( 'NONE', *, *, #21562, .T. ) ;
#12016 = ORIENTED_EDGE ( 'NONE', *, *, #16537, .T. ) ;
#12017 = EDGE_LOOP ( 'NONE', ( #2685, #18704, #21995, #8951 ) ) ;
#12018 = CARTESIAN_POINT ( 'NONE',  ( -0.4417502570507843007, 0.05811937031580000773, -1.934055118110236560 ) ) ;
#12019 = CARTESIAN_POINT ( 'NONE',  ( 0.000000000000000000, 0.000000000000000000, 0.09685039370078740717 ) ) ;
#12020 = AXIS2_PLACEMENT_3D ( 'NONE', #22097, #21693, #26460 ) ;
#12021 = CARTESIAN_POINT ( 'NONE',  ( -0.5511811023622047445, 6.750021727583836750E-17, -1.550196850393700920 ) ) ;
#12022 = CARTESIAN_POINT ( 'NONE',  ( 0.01288382760289894131, 0.1968503937007873850, -3.646653543307086576 ) ) ;
#12023 = ORIENTED_EDGE ( 'NONE', *, *, #23619, .F. ) ;
#12024 = B_SPLINE_CURVE_WITH_KNOTS ( 'NONE', 3,
 ( #6056, #1004, #25389, #12540, #5911, #20487, #1146, #9595 ),
 .UNSPECIFIED., .F., .F.,
 ( 4, 2, 2, 4 ),
 ( 0.000000000000000000, 0.2499999999999998890, 0.4999999999999997780, 1.000000000000000000 ),
 .UNSPECIFIED. ) ;
#12025 = FACE_OUTER_BOUND ( 'NONE', #18987, .T. ) ;
#12026 = ORIENTED_EDGE ( 'NONE', *, *, #17260, .F. ) ;
#12027 = AXIS2_PLACEMENT_3D ( 'NONE', #165, #22561, #17753 ) ;
#12028 = LINE ( 'NONE', #1296, #17049 ) ;
#12029 = CARTESIAN_POINT ( 'NONE',  ( 0.1187185187221477117, -0.3276343780125237637, 0.1589462317918231560 ) ) ;
#12030 = EDGE_CURVE ( 'NONE', #26980, #24440, #17252, .T. ) ;
#12031 = DIRECTION ( 'NONE',  ( 0.000000000000000000, -1.000000000000000000, 0.000000000000000000 ) ) ;
#12032 = CARTESIAN_POINT ( 'NONE',  ( 0.2131049448083992270, -0.5835666837866889667, 0.09685039370078740717 ) ) ;
#12033 = ORIENTED_EDGE ( 'NONE', *, *, #12482, .F. ) ;
#12034 = LINE ( 'NONE', #3249, #27476 ) ;
#12035 = CARTESIAN_POINT ( 'NONE',  ( -0.4856708409191258236, -0.1649135259639268325, -1.550196850393700920 ) ) ;
#12036 = CARTESIAN_POINT ( 'NONE',  ( 0.5511811023622047445, 3.414809992080329023E-17, 0.9202755905511811330 ) ) ;
#12037 = CARTESIAN_POINT ( 'NONE',  ( -0.3362148458988263311, -0.4382482975805425118, 0.9202755905511811330 ) ) ;
#12038 = DIRECTION ( 'NONE',  ( 1.000000000000000000, 0.000000000000000000, 0.000000000000000000 ) ) ;
#12039 = ORIENTED_EDGE ( 'NONE', *, *, #3964, .F. ) ;
#12040 = B_SPLINE_SURFACE_WITH_KNOTS ( 'NONE', 3, 3, ( 
 ( #24047, #5242, #22199, #1018, #13861, #7096, #11326 ),
 ( #19945, #22062, #7365, #15713, #11741, #26854, #15986 ),
 ( #22340, #17934, #20081, #24315, #599, #22484, #20222 ),
 ( #5393, #14013, #26297, #7221, #9192, #2824, #4963 ),
 ( #15840, #736, #26430, #9610, #13577, #9325, #22623 ),
 ( #13436, #2965, #17811, #24444, #24590, #2692, #3112 ),
 ( #18217, #11598, #7507, #26565, #5094, #20503, #9467 ),
 ( #13717, #4820, #11881, #18064, #16133, #26706, #24732 ),
 ( #3243, #9063, #17677, #6963, #15585, #24189, #8081 ) ),
 .UNSPECIFIED., .F., .F., .F.,
 ( 4, 3, 1, 1, 4 ),
 ( 4, 3, 4 ),
 ( -0.9890658252508724990, -0.9807067265327750194, -0.6976453139676740411, -0.5089377055909399816, -0.3202300972142069768 ),
 ( 0.000000000000000000, 1.199999999999999956, 1.211999999999999966 ),
 .UNSPECIFIED. ) ;
#12041 = DIRECTION ( 'NONE',  ( -1.000000000000000000, 1.224646799147353454E-16, 0.000000000000000000 ) ) ;
#12042 = CARTESIAN_POINT ( 'NONE',  ( 0.4889536969035315206, 0.06441834428467128892, -1.569881889763779625 ) ) ;
#12043 = VECTOR ( 'NONE', #13947, 39.37007874015748143 ) ;
#12044 = CARTESIAN_POINT ( 'NONE',  ( 0.4563908000638740581, 0.6818102780177048849, -0.6021022548816948872 ) ) ;
#12045 = CYLINDRICAL_SURFACE ( 'NONE', #3570, 0.4986013261500205074 ) ;
#12046 = ORIENTED_EDGE ( 'NONE', *, *, #2179, .F. ) ;
#12047 = EDGE_CURVE ( 'NONE', #4395, #5951, #2983, .T. ) ;
#12048 = DIRECTION ( 'NONE',  ( 0.000000000000000000, 0.000000000000000000, 1.000000000000000000 ) ) ;
#12049 = DIRECTION ( 'NONE',  ( 0.000000000000000000, -1.000000000000000000, 0.000000000000000000 ) ) ;
#12050 = CARTESIAN_POINT ( 'NONE',  ( 0.000000000000000000, 0.000000000000000000, 0.000000000000000000 ) ) ;
#12051 = CARTESIAN_POINT ( 'NONE',  ( 0.1490609433615242285, -0.2393035190771456711, -0.4144858534716441278 ) ) ;
#12052 = VERTEX_POINT ( 'NONE', #23503 ) ;
#12053 = CARTESIAN_POINT ( 'NONE',  ( -0.3429876364231290164, 0.09193127540154458210, 1.953740157480315043 ) ) ;
#12054 = ORIENTED_EDGE ( 'NONE', *, *, #27465, .F. ) ;
#12055 = CARTESIAN_POINT ( 'NONE',  ( 0.4067073728345788064, -0.2341441294389338956, 0.1992125984251968684 ) ) ;
#12056 = CARTESIAN_POINT ( 'NONE',  ( -0.4932136069632142017, 0.08676634416062008193, 0.09684793308443542803 ) ) ;
#12057 = CARTESIAN_POINT ( 'NONE',  ( 0.01308949271087063437, 0.3147523155727945943, -3.174873752692270124 ) ) ;
#12058 = EDGE_CURVE ( 'NONE', #2317, #5784, #23044, .T. ) ;
#12059 = TOROIDAL_SURFACE ( 'NONE', #27844, 0.4232283464566928832, 0.07677165354330708902 ) ;
#12060 = AXIS2_PLACEMENT_3D ( 'NONE', #15085, #25530, #6320 ) ;
#12061 = DIRECTION ( 'NONE',  ( 1.000000000000000000, 7.017815000000000124E-18, 0.000000000000000000 ) ) ;
#12062 = DIRECTION ( 'NONE',  ( 0.000000000000000000, 0.000000000000000000, 1.000000000000000000 ) ) ;
#12063 = SPHERICAL_SURFACE ( 'NONE', #27148, 0.07677362204724409722 ) ;
#12064 = ORIENTED_EDGE ( 'NONE', *, *, #9346, .F. ) ;
#12065 = CARTESIAN_POINT ( 'NONE',  ( -0.03937007874015747977, 0.5905511811023621549, 0.000000000000000000 ) ) ;
#12066 = DIRECTION ( 'NONE',  ( 0.000000000000000000, 0.000000000000000000, -1.000000000000000000 ) ) ;
#12067 = DIRECTION ( 'NONE',  ( 1.000000000000000000, 0.000000000000000000, 0.000000000000000000 ) ) ;
#12068 = CARTESIAN_POINT ( 'NONE',  ( 0.2842163005028049971, -0.2181214148710412248, -3.115157480314961091 ) ) ;
#12069 = ORIENTED_EDGE ( 'NONE', *, *, #13300, .T. ) ;
#12070 = CARTESIAN_POINT ( 'NONE',  ( 0.4417361510193959506, -0.05819755867303935681, -1.934055118110236338 ) ) ;
#12071 = EDGE_CURVE ( 'NONE', #25742, #24495, #14936, .T. ) ;
#12072 = ORIENTED_EDGE ( 'NONE', *, *, #20343, .F. ) ;
#12073 = ( GEOMETRIC_REPRESENTATION_CONTEXT ( 3 ) GLOBAL_UNCERTAINTY_ASSIGNED_CONTEXT ( ( #18691 ) ) GLOBAL_UNIT_ASSIGNED_CONTEXT ( ( #3059, #16228, #9859 ) ) REPRESENTATION_CONTEXT ( 'NONE', 'WORKASPACE' ) ) ;
#12074 = CIRCLE ( 'NONE', #26917, 0.01377952755905510404 ) ;
#12075 = CARTESIAN_POINT ( 'NONE',  ( -0.4101012214746874163, -0.5753751194595236873, -0.4717551279267843123 ) ) ;
#12076 = DIRECTION ( 'NONE',  ( 0.000000000000000000, 1.000000000000000000, 0.000000000000000000 ) ) ;
#12077 = CARTESIAN_POINT ( 'NONE',  ( -0.5280699926563170443, -0.06957181182498474448, 1.747047244094488194 ) ) ;
#12078 = ORIENTED_EDGE ( 'NONE', *, *, #16004, .F. ) ;
#12079 = CARTESIAN_POINT ( 'NONE',  ( 0.3996755081322992398, 0.4756294029998582307, 0.09684874924366436433 ) ) ;
#12080 = VERTEX_POINT ( 'NONE', #10187 ) ;
#12081 = EDGE_CURVE ( 'NONE', #17434, #14806, #21229, .T. ) ;
#12082 = CARTESIAN_POINT ( 'NONE',  ( 0.2836590635674658412, -0.2488091035916875082, -3.100567304031767168 ) ) ;
#12083 = EDGE_CURVE ( 'NONE', #661, #8860, #5990, .T. ) ;
#12084 = CYLINDRICAL_SURFACE ( 'NONE', #6593, 0.2362204724225640262 ) ;
#12085 = EDGE_CURVE ( 'NONE', #10381, #7546, #19865, .T. ) ;
#12086 = EDGE_LOOP ( 'NONE', ( #13194, #27657 ) ) ;
#12087 = CARTESIAN_POINT ( 'NONE',  ( 0.1110236220424516002, 1.403040230489866364E-17, 0.6299212598425196763 ) ) ;
#12088 = ADVANCED_FACE ( 'NONE', ( #26118, #25464 ), #10337, .T. ) ;
#12089 = CARTESIAN_POINT ( 'NONE',  ( -0.02909913904662018644, 0.4446020952038907681, -1.934055118110236338 ) ) ;
#12090 = ORIENTED_EDGE ( 'NONE', *, *, #14446, .T. ) ;
#12091 = EDGE_LOOP ( 'NONE', ( #9686, #11623, #18619, #18563, #2793, #24065, #16988, #3432, #20037, #9041, #11, #25336, #8753 ) ) ;
#12092 = CARTESIAN_POINT ( 'NONE',  ( -0.3065394984451263460, 0.3644188802919184900, 0.1212655228870160168 ) ) ;
#12093 = CARTESIAN_POINT ( 'NONE',  ( -0.6299212598425196763, 1.087444635826771533, 0.1051828227901515783 ) ) ;
#12094 = CIRCLE ( 'NONE', #13002, 0.1181102362204720091 ) ;
#12095 = VECTOR ( 'NONE', #892, 39.37007874015748143 ) ;
#12096 = CARTESIAN_POINT ( 'NONE',  ( -0.04679574315772456333, -0.3551931031211519874, -3.115157480314960647 ) ) ;
#12097 = CARTESIAN_POINT ( 'NONE',  ( 0.07214943758244279914, -0.5511811023622047445, 0.9202755905511812440 ) ) ;
#12098 = VECTOR ( 'NONE', #776, 39.37007874015748143 ) ;
#12099 = DIRECTION ( 'NONE',  ( 0.000000000000000000, 0.000000000000000000, 1.000000000000000000 ) ) ;
#12100 = CARTESIAN_POINT ( 'NONE',  ( -0.2490711204941342405, 0.9131938423895413770, -0.7142170566240019225 ) ) ;
#12101 = CARTESIAN_POINT ( 'NONE',  ( 0.000000000000000000, 0.000000000000000000, 0.02362204724409448786 ) ) ;
#12102 = CARTESIAN_POINT ( 'NONE',  ( 0.3259357382551448246, -0.08759279594700333793, 1.973425196850394192 ) ) ;
#12104 = CARTESIAN_POINT ( 'NONE',  ( 0.0006615832606325197825, 0.6212594902576319411, 0.09685039370078740717 ) ) ;
#12103 = AXIS2_PLACEMENT_3D ( 'NONE', #18931, #27566, #8209 ) ;
#12105 = CARTESIAN_POINT ( 'NONE',  ( 0.5708661417322835607, 6.829619984160658046E-17, 0.9399606299212598381 ) ) ;
#12106 = CARTESIAN_POINT ( 'NONE',  ( 0.000000000000000000, 0.000000000000000000, 2.504921259842519898 ) ) ;
#12107 = ORIENTED_EDGE ( 'NONE', *, *, #15288, .T. ) ;
#12108 = MANIFOLD_SOLID_BREP ( 'Deep Groove Ball Bearing 20x42x12', #1971 ) ;
#12109 = CARTESIAN_POINT ( 'NONE',  ( 0.5890517850735833560, -0.2103183229436192403, 0.2232855712133572090 ) ) ;
#12110 = CARTESIAN_POINT ( 'NONE',  ( 0.3382184156731939395, -0.3855916753051315538, 1.747047244094488194 ) ) ;
#12111 = CARTESIAN_POINT ( 'NONE',  ( -1.466875984251968630E-17, 0.000000000000000000, -0.4724409448818898127 ) ) ;
#12112 = CARTESIAN_POINT ( 'NONE',  ( 0.4954415918531143714, 0.1327036767659736105, 1.747047244094488194 ) ) ;
#12113 = CIRCLE ( 'NONE', #15728, 0.5322834645669292097 ) ;
#12114 = EDGE_CURVE ( 'NONE', #15651, #25542, #9557, .T. ) ;
#12115 = ORIENTED_EDGE ( 'NONE', *, *, #17686, .F. ) ;
#12116 = AXIS2_PLACEMENT_3D ( 'NONE', #17290, #19823, #26316 ) ;
#12117 = CARTESIAN_POINT ( 'NONE',  ( -0.3334645669291338987, 0.8103892183150610551, -0.9220603341868013336 ) ) ;
#12118 = VERTEX_POINT ( 'NONE', #10476 ) ;
#12119 = AXIS2_PLACEMENT_3D ( 'NONE', #21941, #17281, #2694 ) ;
#12120 = DIRECTION ( 'NONE',  ( 1.000000000000000000, 0.000000000000000000, 0.000000000000000000 ) ) ;
#12121 = FACE_BOUND ( 'NONE', #1617, .T. ) ;
#12122 = ADVANCED_FACE ( 'NONE', ( #7313 ), #10717, .T. ) ;
#12123 = CARTESIAN_POINT ( 'NONE',  ( 0.3015429802576074514, -0.1746717017771027003, 0.1166443193836266407 ) ) ;
#12124 = ORIENTED_EDGE ( 'NONE', *, *, #1474, .T. ) ;
#12125 = CARTESIAN_POINT ( 'NONE',  ( -0.3707612262533165337, -0.3252100150720257932, -1.569881889763779625 ) ) ;
#12126 = VERTEX_POINT ( 'NONE', #10262 ) ;
#12127 = CONTEXT_DEPENDENT_SHAPE_REPRESENTATION ( #278, #13655 ) ;
#12128 = CARTESIAN_POINT ( 'NONE',  ( -0.3574975638436101444, 0.000000000000000000, -3.115157480314960647 ) ) ;
#12129 = CARTESIAN_POINT ( 'NONE',  ( -6.518592411209533944E-17, -0.5322834645669292097, 0.3401574803149606252 ) ) ;
#12130 = DIRECTION ( 'NONE',  ( 0.000000000000000000, -1.000000000000000000, 0.000000000000000000 ) ) ;
#12131 = AXIS2_PLACEMENT_3D ( 'NONE', #14237, #22843, #7580 ) ;
#12132 = AXIS2_PLACEMENT_3D ( 'NONE', #9306, #4667, #7348 ) ;
#12133 = ORIENTED_EDGE ( 'NONE', *, *, #4241, .F. ) ;
#12134 = CARTESIAN_POINT ( 'NONE',  ( 0.5869493968219645641, -0.2133897621573078718, -0.3696019098714952711 ) ) ;
#12135 = CIRCLE ( 'NONE', #14879, 0.7552056691767480290 ) ;
#12136 = UNCERTAINTY_MEASURE_WITH_UNIT (LENGTH_MEASURE( 1.000000000000000082E-05 ), #10314, 'distance_accuracy_value', 'NONE') ;
#12137 = FACE_OUTER_BOUND ( 'NONE', #8092, .T. ) ;
#12138 = FACE_OUTER_BOUND ( 'NONE', #2532, .T. ) ;
#12139 = CARTESIAN_POINT ( 'NONE',  ( -0.6042317347120136350, -0.1855048251218045230, 0.2228014207307441874 ) ) ;
#12140 = CARTESIAN_POINT ( 'NONE',  ( 0.5708661417322835607, 6.829619984160658046E-17, 0.9399606299212598381 ) ) ;
#12141 = COLOUR_RGB ( '', 0.66274510, 0.83137255, 0.94901961) ;
#12142 = DIRECTION ( 'NONE',  ( -1.000000000000000000, 0.000000000000000000, 0.000000000000000000 ) ) ;
#12143 = DIRECTION ( 'NONE',  ( 0.000000000000000000, 0.000000000000000000, -1.000000000000000000 ) ) ;
#12144 = ORIENTED_EDGE ( 'NONE', *, *, #19914, .T. ) ;
#12145 = ORIENTED_EDGE ( 'NONE', *, *, #24591, .T. ) ;
#12146 = EDGE_CURVE ( 'NONE', #5072, #21621, #12382, .T. ) ;
#12147 = AXIS2_PLACEMENT_3D ( 'NONE', #7460, #20746, #13972 ) ;
#12148 = EDGE_LOOP ( 'NONE', ( #22079, #6928, #13642, #27, #4314, #15946 ) ) ;
#12149 = DIRECTION ( 'NONE',  ( 1.000000000000000000, 0.000000000000000000, 0.000000000000000000 ) ) ;
#12150 = LINE ( 'NONE', #25437, #1283 ) ;
#12151 = APPLICATION_CONTEXT ( 'automotive_design' ) ;
#12152 = DIRECTION ( 'NONE',  ( 0.000000000000000000, 0.000000000000000000, -1.000000000000000000 ) ) ;
#12153 = CARTESIAN_POINT ( 'NONE',  ( 0.4954247181591565075, 0.1327957795770679794, -1.550196850393700476 ) ) ;
#12154 = ORIENTED_EDGE ( 'NONE', *, *, #862, .F. ) ;
#12155 = DIRECTION ( 'NONE',  ( 1.000000000000000000, 0.000000000000000000, 0.000000000000000000 ) ) ;
#12156 = DIRECTION ( 'NONE',  ( 0.000000000000000000, 0.000000000000000000, 1.000000000000000000 ) ) ;
#12157 = DIRECTION ( 'NONE',  ( 0.000000000000000000, 0.000000000000000000, -1.000000000000000000 ) ) ;
#12158 = CARTESIAN_POINT ( 'NONE',  ( -0.4857053587577855880, -0.1648264847746778727, -1.550196850393700920 ) ) ;
#12159 = EDGE_CURVE ( 'NONE', #22507, #26151, #1841, .T. ) ;
#12160 = CARTESIAN_POINT ( 'NONE',  ( -0.1710938124795999826, -0.4706537664821763833, 0.2574827755769819038 ) ) ;
#12161 = VERTEX_POINT ( 'NONE', #25671 ) ;
#12162 = CARTESIAN_POINT ( 'NONE',  ( -0.6478824768902187170, 0.1135474080053010398, 0.2081850588238823851 ) ) ;
#12163 = EDGE_LOOP ( 'NONE', ( #14445, #21411, #9961, #21902 ) ) ;
#12164 = CARTESIAN_POINT ( 'NONE',  ( -0.2165354330708661457, 1.112204724409448842, 1.362057955744595713E-16 ) ) ;
#12165 = AXIS2_PLACEMENT_3D ( 'NONE', #9502, #12061, #7400 ) ;
#12166 = CARTESIAN_POINT ( 'NONE',  ( -0.1288360683667815199, -0.3544784926413476200, 0.1992150590373740204 ) ) ;
#12167 = AXIS2_PLACEMENT_3D ( 'NONE', #10712, #8733, #292 ) ;
#12168 = CARTESIAN_POINT ( 'NONE',  ( -0.5335524835332036142, 0.1429116519061177371, 0.9399606299212598381 ) ) ;
#12169 = CARTESIAN_POINT ( 'NONE',  ( -0.3174445073355823266, -0.1826860508809280137, 0.1910323753023780158 ) ) ;
#12170 = CARTESIAN_POINT ( 'NONE',  ( -0.1257482708741702870, -0.3439950301908584196, 0.1910323753022282467 ) ) ;
#12171 = ORIENTED_EDGE ( 'NONE', *, *, #26613, .F. ) ;
#12172 = DIRECTION ( 'NONE',  ( 0.000000000000000000, -1.000000000000000000, 0.000000000000000000 ) ) ;
#12173 = ( CONVERSION_BASED_UNIT ( 'INCH', #26723 ) LENGTH_UNIT ( ) NAMED_UNIT ( #16264 ) ) ;
#12174 = CIRCLE ( 'NONE', #61, 0.5511811023622047445 ) ;
#12175 = ORIENTED_EDGE ( 'NONE', *, *, #13139, .F. ) ;
#12176 = CARTESIAN_POINT ( 'NONE',  ( -0.1918813796216842782, -0.5271897577243779276, 0.1771653543307086520 ) ) ;
#12177 = CARTESIAN_POINT ( 'NONE',  ( 0.1379038425970668946, 0.5144793533648593931, 1.747047244094488194 ) ) ;
#12178 = EDGE_CURVE ( 'NONE', #16783, #9781, #5910, .T. ) ;
#12179 = EDGE_LOOP ( 'NONE', ( #21943, #17068, #27719, #6755 ) ) ;
#12180 = EDGE_CURVE ( 'NONE', #17997, #22192, #497, .T. ) ;
#12181 = DIRECTION ( 'NONE',  ( -0.9236347588935202024, 0.3832738344365670957, 0.000000000000000000 ) ) ;
#12182 = DIRECTION ( 'NONE',  ( 1.000000000000000000, 0.000000000000000000, 0.000000000000000000 ) ) ;
#12183 = ORIENTED_EDGE ( 'NONE', *, *, #17152, .T. ) ;
#12184 = DIRECTION ( 'NONE',  ( 1.000000000000000000, 0.000000000000000000, 0.000000000000000000 ) ) ;
#12185 = CARTESIAN_POINT ( 'NONE',  ( -0.5187889641967551313, -0.1190953285357212593, 0.1322834645669291320 ) ) ;
#12186 = ORIENTED_EDGE ( 'NONE', *, *, #14718, .F. ) ;
#12187 = CARTESIAN_POINT ( 'NONE',  ( 6.026805113914139867E-17, 0.4724409448818898127, 0.4921259842519685179 ) ) ;
#12188 = EDGE_LOOP ( 'NONE', ( #5238, #20973, #20535, #9395 ) ) ;
#12189 = CYLINDRICAL_SURFACE ( 'NONE', #17919, 0.6889763779527560139 ) ;
#12190 = CIRCLE ( 'NONE', #21683, 0.03937007874015744507 ) ;
#12191 = CARTESIAN_POINT ( 'NONE',  ( 0.3174445073395564254, -0.1826860508832116869, 0.08455817587528674517 ) ) ;
#12192 = CARTESIAN_POINT ( 'NONE',  ( 0.3013593406941988406, 0.3597456680659192330, 0.07637630773773071424 ) ) ;
#12193 = DIRECTION ( 'NONE',  ( 0.000000000000000000, -1.000000000000000000, 0.000000000000000000 ) ) ;
#12194 = LINE ( 'NONE', #23089, #20361 ) ;
#12195 = ORIENTED_EDGE ( 'NONE', *, *, #24359, .F. ) ;
#12196 = DIRECTION ( 'NONE',  ( 1.000000000000000000, 0.000000000000000000, 0.000000000000000000 ) ) ;
#12197 = CARTESIAN_POINT ( 'NONE',  ( 0.000000000000000000, 0.000000000000000000, -6.283251968503937502E-17 ) ) ;
#12198 = PRESENTATION_LAYER_ASSIGNMENT (  '', '', ( #22119 ) ) ;
#12199 = CARTESIAN_POINT ( 'NONE',  ( 0.000000000000000000, 0.000000000000000000, -4.330708661417323135 ) ) ;
#12200 = CARTESIAN_POINT ( 'NONE',  ( 0.5379714048901780288, 6.588249590315613132E-17, -0.2342519685039370358 ) ) ;
#12201 = MANIFOLD_SOLID_BREP ( 'Bearing Cup', #23648 ) ;
#12202 = CARTESIAN_POINT ( 'NONE',  ( -0.3574975638436101444, -0.02348089843015294109, -3.115157480314960203 ) ) ;
#12203 = CARTESIAN_POINT ( 'NONE',  ( 0.1259842519685039353, 0.000000000000000000, 0.1181010187644645354 ) ) ;
#12204 = CARTESIAN_POINT ( 'NONE',  ( 0.4270824798167637826, -0.2466292688015195855, -1.569881889763779625 ) ) ;
#12205 = VERTEX_POINT ( 'NONE', #6598 ) ;
#12206 = EDGE_CURVE ( 'NONE', #23369, #6563, #394, .T. ) ;
#12207 = CARTESIAN_POINT ( 'NONE',  ( -0.05819755867304135522, -0.4417361510194244278, -1.934055118110236338 ) ) ;
#12208 = B_SPLINE_CURVE_WITH_KNOTS ( 'NONE', 3,
 ( #1691, #23606, #25427, #14729 ),
 .UNSPECIFIED., .F., .F.,
 ( 4, 4 ),
 ( 0.9046454396443728285, 0.9061502038671860326 ),
 .UNSPECIFIED. ) ;
#12209 = ORIENTED_EDGE ( 'NONE', *, *, #8880, .T. ) ;
#12210 = VERTEX_POINT ( 'NONE', #23568 ) ;
#12211 = ORIENTED_EDGE ( 'NONE', *, *, #12829, .F. ) ;
#12213 = ORIENTED_EDGE ( 'NONE', *, *, #8260, .F. ) ;
#12212 = ADVANCED_FACE ( 'NONE', ( #12941 ), #15091, .F. ) ;
#12214 = B_SPLINE_CURVE_WITH_KNOTS ( 'NONE', 3,
 ( #13995, #7081, #9746, #15700, #2682, #24172, #13424, #13565 ),
 .UNSPECIFIED., .F., .F.,
 ( 4, 2, 2, 4 ),
 ( 0.5000000000000000000, 0.7499999999999997780, 0.8749999999999998890, 1.000000000000000000 ),
 .UNSPECIFIED. ) ;
#12215 = CARTESIAN_POINT ( 'NONE',  ( 0.5604501195244573353, 0.4479362078561491822, 0.3122824329334484283 ) ) ;
#12216 = LINE ( 'NONE', #16735, #9516 ) ;
#12217 = CARTESIAN_POINT ( 'NONE',  ( -0.3512268162760389667, -0.4004221243553605092, 1.747047244094488194 ) ) ;
#12218 = ORIENTED_EDGE ( 'NONE', *, *, #13203, .T. ) ;
#12219 = CARTESIAN_POINT ( 'NONE',  ( 0.3990005999895503419, 0.4761957181735173017, 0.09684874924366436433 ) ) ;
#12220 = VERTEX_POINT ( 'NONE', #2482 ) ;
#12221 = VECTOR ( 'NONE', #16324, 39.37007874015748143 ) ;
#12222 = CARTESIAN_POINT ( 'NONE',  ( 0.02464264302293787262, 0.3765118517642104257, -3.100567304031763172 ) ) ;
#12223 = DIRECTION ( 'NONE',  ( 0.000000000000000000, 0.000000000000000000, -1.000000000000000000 ) ) ;
#12224 = CARTESIAN_POINT ( 'NONE',  ( -0.4921259842519685179, 6.026805113914139867E-17, -1.934055118110236338 ) ) ;
#12225 = CARTESIAN_POINT ( 'NONE',  ( -0.09187177619658884464, -0.3429980251342297226, 1.953740157480315043 ) ) ;
#12226 = ORIENTED_EDGE ( 'NONE', *, *, #11568, .F. ) ;
#12227 = CARTESIAN_POINT ( 'NONE',  ( -0.6065227633320124934, -0.1124154687194963698, -0.2439881145186360845 ) ) ;
#12229 = CARTESIAN_POINT ( 'NONE',  ( 0.5230301363770953893, -0.1775991818008574585, 0.9399606299212598381 ) ) ;
#12228 = CARTESIAN_POINT ( 'NONE',  ( 4.701028524955307180E-18, 0.4232283464566928832, 0.2145688976377952695 ) ) ;
#12230 = LINE ( 'NONE', #26398, #18006 ) ;
#12231 = ORIENTED_EDGE ( 'NONE', *, *, #27863, .F. ) ;
#12232 = ORIENTED_EDGE ( 'NONE', *, *, #4565, .T. ) ;
#12233 = DIRECTION ( 'NONE',  ( 0.000000000000000000, 0.000000000000000000, 1.000000000000000000 ) ) ;
#12234 = CARTESIAN_POINT ( 'NONE',  ( -0.4895985792973480133, 0.000000000000000000, 0.000000000000000000 ) ) ;
#12235 = B_SPLINE_CURVE_WITH_KNOTS ( 'NONE', 3,
 ( #21255, #17022, #25629, #6668, #9043, #24164, #4799, #13416, #20061, #22739 ),
 .UNSPECIFIED., .F., .F.,
 ( 4, 2, 2, 2, 4 ),
 ( 0.000000000000000000, 0.2500000000000001665, 0.5000000000000003331, 0.7500000000000001110, 1.000000000000000000 ),
 .UNSPECIFIED. ) ;
#12236 = CIRCLE ( 'NONE', #11787, 0.02362204724409448092 ) ;
#12237 = CARTESIAN_POINT ( 'NONE',  ( 0.2693339498142349187, -0.2362439534887297299, -3.115157480314960647 ) ) ;
#12238 = CARTESIAN_POINT ( 'NONE',  ( -0.4407612517155323206, -0.3387265385688508768, 0.9202755905511813550 ) ) ;
#12239 = CARTESIAN_POINT ( 'NONE',  ( 0.1520645003680120011, 0.2938566582910456804, -0.3972204521033417812 ) ) ;
#12240 = FACE_OUTER_BOUND ( 'NONE', #22302, .T. ) ;
#12241 = ADVANCED_FACE ( 'NONE', ( #11105 ), #19890, .F. ) ;
#12242 = EDGE_CURVE ( 'NONE', #6891, #2437, #7715, .T. ) ;
#12243 = FACE_OUTER_BOUND ( 'NONE', #23904, .T. ) ;
#12244 = EDGE_CURVE ( 'NONE', #20990, #21275, #23863, .T. ) ;
#12245 = ORIENTED_EDGE ( 'NONE', *, *, #701, .F. ) ;
#12246 = CARTESIAN_POINT ( 'NONE',  ( -0.4986013261500205074, 0.000000000000000000, -0.1756889763779527769 ) ) ;
#12247 = LINE ( 'NONE', #16356, #7578 ) ;
#12248 = EDGE_CURVE ( 'NONE', #27195, #14336, #26645, .T. ) ;
#12249 = DIRECTION ( 'NONE',  ( -1.000000000000000000, 0.000000000000000000, 0.000000000000000000 ) ) ;
#12250 = CARTESIAN_POINT ( 'NONE',  ( 0.4612490782034816550, -0.2663596103035388296, 1.747047244094488194 ) ) ;
#12251 = CARTESIAN_POINT ( 'NONE',  ( 0.5118110236220472231, -0.03349795313260760937, 1.766732283464566899 ) ) ;
#12252 = ORIENTED_EDGE ( 'NONE', *, *, #16658, .F. ) ;
#12253 = CIRCLE ( 'NONE', #529, 0.1181102362204718703 ) ;
#12254 = ORIENTED_EDGE ( 'NONE', *, *, #24754, .F. ) ;
#12255 = CARTESIAN_POINT ( 'NONE',  ( 0.1669561253490893793, -0.4569961989603250618, 0.1075369453269351266 ) ) ;
#12256 = EDGE_LOOP ( 'NONE', ( #4491, #23321, #15253, #5381 ) ) ;
#12257 = CARTESIAN_POINT ( 'NONE',  ( 0.3785000865561056194, 0.3010298976871484400, 0.2008762816001854468 ) ) ;
#12258 = DIRECTION ( 'NONE',  ( 0.000000000000000000, 0.000000000000000000, -1.000000000000000000 ) ) ;
#12259 = CARTESIAN_POINT ( 'NONE',  ( 0.3611077606078542668, 0.7441461625961331983, -0.7153708716273008417 ) ) ;
#12260 = FACE_OUTER_BOUND ( 'NONE', #25067, .T. ) ;
#12261 = ORIENTED_EDGE ( 'NONE', *, *, #25033, .T. ) ;
#12262 = CIRCLE ( 'NONE', #26235, 0.5511811023622047445 ) ;
#12263 = ORIENTED_EDGE ( 'NONE', *, *, #14355, .F. ) ;
#12264 = AXIS2_PLACEMENT_3D ( 'NONE', #19964, #620, #17830 ) ;
#12265 = CARTESIAN_POINT ( 'NONE',  ( 0.4889536969034952718, -0.06441834428466330920, -1.550196850393700920 ) ) ;
#12266 = CARTESIAN_POINT ( 'NONE',  ( 2.066929133858267598, 0.4724409448818898127, 0.000000000000000000 ) ) ;
#12267 = ORIENTED_EDGE ( 'NONE', *, *, #14581, .F. ) ;
#12268 = CONTEXT_DEPENDENT_SHAPE_REPRESENTATION ( #12694, #1045 ) ;
#12269 = CARTESIAN_POINT ( 'NONE',  ( 0.000000000000000000, 0.000000000000000000, -4.291338582656260670 ) ) ;
#12270 = CARTESIAN_POINT ( 'NONE',  ( 0.2120693917185543231, -0.5839438448129543602, 0.09684874924366436433 ) ) ;
#12271 = CARTESIAN_POINT ( 'NONE',  ( 0.07874015748031495954, 0.04546065111729338803, -0.4724409448818898127 ) ) ;
#12272 = CARTESIAN_POINT ( 'NONE',  ( -0.4622285577935968948, 0.08111201067590709246, 0.1992142434433716580 ) ) ;
#12273 = PRODUCT_DEFINITION_SHAPE ( 'NONE', 'NONE',  #2378 ) ;
#12274 = EDGE_CURVE ( 'NONE', #240, #2204, #5928, .T. ) ;
#12275 = AXIS2_PLACEMENT_3D ( 'NONE', #5534, #14596, #23198 ) ;
#12276 = EDGE_LOOP ( 'NONE', ( #24684, #17074, #15910, #6676 ) ) ;
#12277 = CARTESIAN_POINT ( 'NONE',  ( -0.3214446924536846772, 0.3840069416942866742, 0.2574803149606298969 ) ) ;
#12278 = EDGE_CURVE ( 'NONE', #22294, #16690, #4597, .T. ) ;
#12279 = DIRECTION ( 'NONE',  ( 0.000000000000000000, 1.000000000000000000, 0.000000000000000000 ) ) ;
#12280 = DIRECTION ( 'NONE',  ( 0.000000000000000000, 0.000000000000000000, 1.000000000000000000 ) ) ;
#12281 = CARTESIAN_POINT ( 'NONE',  ( -0.06181127634704723650, -1.564461769117756029, 2.145669291338582862 ) ) ;
#12282 = CIRCLE ( 'NONE', #5983, 0.7165354330708662012 ) ;
#12283 = CARTESIAN_POINT ( 'NONE',  ( -0.4326303163632846394, -0.8192757351588600967, -0.05768471019755529866 ) ) ;
#12284 = EDGE_CURVE ( 'NONE', #25761, #6278, #9957, .T. ) ;
#12285 = CARTESIAN_POINT ( 'NONE',  ( 0.2128972891168984249, -0.5836425148029299459, 0.2574819594177527593 ) ) ;
#12286 = CARTESIAN_POINT ( 'NONE',  ( -0.3543307086367249448, 4.339299681715786259E-17, -4.330708661417323135 ) ) ;
#12287 = EDGE_CURVE ( 'NONE', #22576, #21648, #15112, .T. ) ;
#12288 = ORIENTED_EDGE ( 'NONE', *, *, #12663, .F. ) ;
#12289 = ORIENTED_EDGE ( 'NONE', *, *, #14410, .F. ) ;
#12290 = FACE_OUTER_BOUND ( 'NONE', #2120, .T. ) ;
#12291 = CIRCLE ( 'NONE', #1930, 0.4921259842519685179 ) ;
#12292 = ORIENTED_EDGE ( 'NONE', *, *, #1538, .F. ) ;
#12293 = DIRECTION ( 'NONE',  ( 0.000000000000000000, 0.000000000000000000, -1.000000000000000000 ) ) ;
#12294 = FACE_BOUND ( 'NONE', #520, .T. ) ;
#12295 = FACE_OUTER_BOUND ( 'NONE', #7293, .T. ) ;
#12296 = DIMENSIONAL_EXPONENTS ( 1.000000000000000000, 0.000000000000000000, 0.000000000000000000, 0.000000000000000000, 0.000000000000000000, 0.000000000000000000, 0.000000000000000000 ) ;
#12297 = VERTEX_POINT ( 'NONE', #4336 ) ;
#12298 = DIRECTION ( 'NONE',  ( 0.000000000000000000, 1.000000000000000000, 0.000000000000000000 ) ) ;
#12299 = ORIENTED_EDGE ( 'NONE', *, *, #17135, .T. ) ;
#12300 = CIRCLE ( 'NONE', #23147, 0.6881889763779527325 ) ;
#12301 = DIRECTION ( 'NONE',  ( -0.000000000000000000, 0.000000000000000000, -1.000000000000000000 ) ) ;
#12302 = CARTESIAN_POINT ( 'NONE',  ( -0.1968503937007874127, -5.802129921259842692E-18, 0.000000000000000000 ) ) ;
#12303 = CARTESIAN_POINT ( 'NONE',  ( 0.1285103288269283661, -0.3545966721392122545, 0.1992125984251968684 ) ) ;
#12304 = CARTESIAN_POINT ( 'NONE',  ( 0.3031496062992122820, 3.712511950171106268E-17, -0.03543307086614204404 ) ) ;
#12305 = VERTEX_POINT ( 'NONE', #21847 ) ;
#12306 = DIRECTION ( 'NONE',  ( 0.000000000000000000, 0.000000000000000000, 1.000000000000000000 ) ) ;
#12307 = DIRECTION ( 'NONE',  ( -1.000000000000000000, 1.224646799147353454E-16, 0.000000000000000000 ) ) ;
#12308 = CARTESIAN_POINT ( 'NONE',  ( 0.2660793235464212203, 0.2041304421298323901, 1.953740157480315043 ) ) ;
#12309 = CARTESIAN_POINT ( 'NONE',  ( 0.000000000000000000, 0.000000000000000000, 0.07637795275590551769 ) ) ;
#12310 = EDGE_CURVE ( 'NONE', #11643, #19740, #10967, .T. ) ;
#12311 = DIRECTION ( 'NONE',  ( 0.000000000000000000, 0.000000000000000000, -1.000000000000000000 ) ) ;
#12312 = CARTESIAN_POINT ( 'NONE',  ( 0.6299212598425196763, -1.895600393700787470E-35, 0.000000000000000000 ) ) ;
#12313 = CIRCLE ( 'NONE', #1486, 0.1673228346456692994 ) ;
#12314 = B_SPLINE_CURVE_WITH_KNOTS ( 'NONE', 3,
 ( #299, #19754, #23731, #26112, #422, #24259 ),
 .UNSPECIFIED., .F., .F.,
 ( 4, 2, 4 ),
 ( 1.162880698919835920, 1.164573402063409979, 1.166266105206984038 ),
 .UNSPECIFIED. ) ;
#12315 = CARTESIAN_POINT ( 'NONE',  ( 0.1429116519061152946, -0.5335524835331961757, 0.9399606299212598381 ) ) ;
#12316 = DIRECTION ( 'NONE',  ( 0.000000000000000000, 0.000000000000000000, -1.000000000000000000 ) ) ;
#12317 = CARTESIAN_POINT ( 'NONE',  ( -0.3263749705684267921, -0.1890319631540330891, 0.1992125984251968684 ) ) ;
#12318 = EDGE_LOOP ( 'NONE', ( #17872, #13213, #10063, #27416 ) ) ;
#12319 = CARTESIAN_POINT ( 'NONE',  ( 0.0005789221761214173069, 0.4692909815006417462, 0.07637795275590551769 ) ) ;
#12320 = ADVANCED_FACE ( 'NONE', ( #14214 ), #27585, .F. ) ;
#12321 = PRESENTATION_STYLE_ASSIGNMENT (( #3994 ) ) ;
#12323 = ORIENTED_EDGE ( 'NONE', *, *, #10010, .T. ) ;
#12324 = DIRECTION ( 'NONE',  ( 0.000000000000000000, -1.000000000000000000, 0.000000000000000000 ) ) ;
#12325 = DIRECTION ( 'NONE',  ( -1.000000000000000000, 0.000000000000000000, 0.000000000000000000 ) ) ;
#12326 = CARTESIAN_POINT ( 'NONE',  ( -0.2712027394948519632, -0.3535065162672669792, -1.934055118110236338 ) ) ;
#12327 = CARTESIAN_POINT ( 'NONE',  ( -0.5905511811023621549, 7.232166136696967594E-17, 0.9399606299212598381 ) ) ;
#12328 = CARTESIAN_POINT ( 'NONE',  ( -0.06690297524288160713, 0.5085287184739378796, -1.550196850393700476 ) ) ;
#12329 = EDGE_LOOP ( 'NONE', ( #1441, #11281 ) ) ;
#12330 = AXIS2_PLACEMENT_3D ( 'NONE', #24886, #18368, #12038 ) ;
#12331 = DIRECTION ( 'NONE',  ( 1.000000000000000000, 0.000000000000000000, 0.000000000000000000 ) ) ;
#12332 = ORIENTED_EDGE ( 'NONE', *, *, #19290, .T. ) ;
#12333 = AXIS2_PLACEMENT_3D ( 'NONE', #9905, #16978, #25304 ) ;
#12334 = CARTESIAN_POINT ( 'NONE',  ( -0.4167985568850881561, 0.07349283109919310664, 0.1377952755905511861 ) ) ;
#12335 = CARTESIAN_POINT ( 'NONE',  ( -0.5677492016568244093, -0.6030946203083737966, -0.9382345488188125193 ) ) ;
#12336 = FACE_BOUND ( 'NONE', #22195, .T. ) ;
#12337 = CARTESIAN_POINT ( 'NONE',  ( -0.3607825703577880461, 0.06309631803640179670, 0.08455817587900750498 ) ) ;
#12338 = ORIENTED_EDGE ( 'NONE', *, *, #22297, .T. ) ;
#12339 = CARTESIAN_POINT ( 'NONE',  ( 0.7874015748031496509, -0.4579607000970866149, -0.1931355542581366103 ) ) ;
#12340 = VERTEX_POINT ( 'NONE', #22820 ) ;
#12341 = DIRECTION ( 'NONE',  ( 0.000000000000000000, 0.000000000000000000, 1.000000000000000000 ) ) ;
#12343 = ADVANCED_FACE ( 'NONE', ( #791 ), #15417, .F. ) ;
#12342 = CIRCLE ( 'NONE', #3769, 0.06889763779527552368 ) ;
#12344 = CARTESIAN_POINT ( 'NONE',  ( 0.4130706566799093316, -0.3346769814300175616, 0.5796775359605756961 ) ) ;
#12345 = AXIS2_PLACEMENT_3D ( 'NONE', #22887, #16381, #19049 ) ;
#12346 = FILL_AREA_STYLE_COLOUR ( '', #19749 ) ;
#12347 = EDGE_CURVE ( 'NONE', #24512, #15164, #19129, .T. ) ;
#12348 = VERTEX_POINT ( 'NONE', #7275 ) ;
#12349 = AXIS2_PLACEMENT_3D ( 'NONE', #27079, #7727, #24941 ) ;
#12350 = CARTESIAN_POINT ( 'NONE',  ( 0.1970259548082107792, -0.3996230174612653285, -1.934055118110236338 ) ) ;
#12351 = EDGE_CURVE ( 'NONE', #11643, #22824, #3187, .T. ) ;
#12352 = CIRCLE ( 'NONE', #1528, 0.1003956692913385990 ) ;
#12353 = CARTESIAN_POINT ( 'NONE',  ( 0.000000000000000000, 0.07874015748031495954, -1.377952755905512472 ) ) ;
#12354 = ORIENTED_EDGE ( 'NONE', *, *, #7891, .T. ) ;
#12355 = VERTEX_POINT ( 'NONE', #932 ) ;
#12356 = CARTESIAN_POINT ( 'NONE',  ( -0.5935113537020059171, -0.1684283806775520032, -0.09332418187737165360 ) ) ;
#12357 = CARTESIAN_POINT ( 'NONE',  ( 0.3382184156731939395, -0.3855916753051315538, 1.747047244094488194 ) ) ;
#12358 = DIRECTION ( 'NONE',  ( -0.000000000000000000, -0.000000000000000000, -1.000000000000000000 ) ) ;
#12359 = ORIENTED_EDGE ( 'NONE', *, *, #13812, .T. ) ;
#12360 = AXIS2_PLACEMENT_3D ( 'NONE', #27589, #6531, #15161 ) ;
#12361 = CARTESIAN_POINT ( 'NONE',  ( -0.1668516812751421607, 0.3384212623783116602, -3.100567304031759175 ) ) ;
#12362 = AXIS2_PLACEMENT_3D ( 'NONE', #20394, #26743, #11631 ) ;
#12363 = CARTESIAN_POINT ( 'NONE',  ( 0.2262947209289010442, -0.4714317853940108716, 0.1392975274349756987 ) ) ;
#12364 = CARTESIAN_POINT ( 'NONE',  ( -0.5383630292499967940, 0.4286833100733401514, 0.1322818203437346463 ) ) ;
#12365 = CARTESIAN_POINT ( 'NONE',  ( 0.1570220809524492389, -0.3184841198566451537, 1.953740157480315043 ) ) ;
#12366 = VERTEX_POINT ( 'NONE', #2881 ) ;
#12367 = CARTESIAN_POINT ( 'NONE',  ( -0.4612762626262458809, -0.4482319504133971400, -0.3686284328691009637 ) ) ;
#12368 = CARTESIAN_POINT ( 'NONE',  ( 8.810208661417323492E-17, -4.420669291338583154E-18, 0.000000000000000000 ) ) ;
#12370 = CARTESIAN_POINT ( 'NONE',  ( 0.4539000224941339701, 0.3482225189666781073, 0.9399606299212598381 ) ) ;
#12369 = CARTESIAN_POINT ( 'NONE',  ( -0.2313841235333770063, -0.3010840436257778419, -3.100567304031762284 ) ) ;
#12371 = DIRECTION ( 'NONE',  ( -1.000000000000000000, 0.000000000000000000, 0.000000000000000000 ) ) ;
#12372 = ORIENTED_EDGE ( 'NONE', *, *, #4119, .F. ) ;
#12373 = ORIENTED_EDGE ( 'NONE', *, *, #22284, .T. ) ;
#12374 = LINE ( 'NONE', #25086, #2783 ) ;
#12375 = DIRECTION ( 'NONE',  ( 1.000000000000000000, 0.000000000000000000, 0.000000000000000000 ) ) ;
#12376 = CIRCLE ( 'NONE', #234, 0.7874015748031496509 ) ;
#12377 = ( BOUNDED_CURVE ( )  B_SPLINE_CURVE ( 2, ( #18620, #3648, #5937 ),
 .UNSPECIFIED., .F., .F. ) 
 B_SPLINE_CURVE_WITH_KNOTS ( ( 3, 3 ),
 ( 0.000000000000000000, 0.5842180690389588982 ),
 .UNSPECIFIED. ) 
 CURVE ( )  GEOMETRIC_REPRESENTATION_ITEM ( )  RATIONAL_B_SPLINE_CURVE ( ( 1.000000000000000000, 1.154700538379253905, 1.000000000000000000 ) ) 
 REPRESENTATION_ITEM ( '' )  ) ;
#12378 = CARTESIAN_POINT ( 'NONE',  ( -0.3574975638436101444, 0.000000000000000000, -3.115157480314960647 ) ) ;
#12379 = DIRECTION ( 'NONE',  ( 0.000000000000000000, 0.000000000000000000, 1.000000000000000000 ) ) ;
#12380 = CARTESIAN_POINT ( 'NONE',  ( 0.1518453843511950729, 0.2938239883646059369, -0.3972446186700991921 ) ) ;
#12381 = CARTESIAN_POINT ( 'NONE',  ( -8.632637795275590524E-16, -1.576771653543307172, 9.184850993605150903E-17 ) ) ;
#12382 = B_SPLINE_CURVE_WITH_KNOTS ( 'NONE', 3,
 ( #27377, #19024, #25535, #7885, #16634, #23142, #8308, #16490, #25249, #21297 ),
 .UNSPECIFIED., .F., .F.,
 ( 4, 2, 2, 2, 4 ),
 ( 0.5000000000000000000, 0.6250000000000000000, 0.7500000000000000000, 0.8750000000000000000, 1.000000000000000000 ),
 .UNSPECIFIED. ) ;
#12383 = EDGE_CURVE ( 'NONE', #4894, #10695, #9377, .T. ) ;
#12384 = FACE_OUTER_BOUND ( 'NONE', #21091, .T. ) ;
#12385 = AXIS2_PLACEMENT_3D ( 'NONE', #9010, #2653, #19896 ) ;
#12386 = DIRECTION ( 'NONE',  ( 1.000000000000000000, 0.000000000000000000, 0.000000000000000000 ) ) ;
#12387 = CIRCLE ( 'NONE', #8328, 0.4692913385826771866 ) ;
#12388 = CARTESIAN_POINT ( 'NONE',  ( -4.821283464566928349E-18, 0.000000000000000000, -0.3779527559055118058 ) ) ;
#12389 = ORIENTED_EDGE ( 'NONE', *, *, #16621, .T. ) ;
#12390 = DIRECTION ( 'NONE',  ( 0.000000000000000000, 0.000000000000000000, -1.000000000000000000 ) ) ;
#12391 = DIRECTION ( 'NONE',  ( 0.000000000000000000, 0.000000000000000000, -1.000000000000000000 ) ) ;
#12392 = CARTESIAN_POINT ( 'NONE',  ( -0.4688657571743830577, 0.08326155277092069096, 0.1212655228864951557 ) ) ;
#12393 = CARTESIAN_POINT ( 'NONE',  ( 0.6055690743987126590, 0.2581485381169799642, -0.4471263839182408883 ) ) ;
#12394 = DIRECTION ( 'NONE',  ( 0.000000000000000000, 0.000000000000000000, 1.000000000000000000 ) ) ;
#12395 = SURFACE_STYLE_USAGE ( .BOTH. , #3623 ) ;
#12396 = CARTESIAN_POINT ( 'NONE',  ( -0.2256062985779239694, -0.6178563876543621269, 0.2081850588299369031 ) ) ;
#12397 = CARTESIAN_POINT ( 'NONE',  ( 0.4600326175560603970, 0.2268096725222477072, 1.747047244094488194 ) ) ;
#12398 = VECTOR ( 'NONE', #26763, 39.37007874015748143 ) ;
#12399 = ORIENTED_EDGE ( 'NONE', *, *, #12081, .T. ) ;
#12400 = ORIENTED_EDGE ( 'NONE', *, *, #19654, .F. ) ;
#12401 = CARTESIAN_POINT ( 'NONE',  ( 0.1634143070181317270, -0.4472844159275946030, 0.1212655228078316633 ) ) ;
#12402 = ORIENTED_EDGE ( 'NONE', *, *, #16442, .F. ) ;
#12403 = CARTESIAN_POINT ( 'NONE',  ( 0.5905511811023621549, 0.000000000000000000, 0.000000000000000000 ) ) ;
#12404 = CARTESIAN_POINT ( 'NONE',  ( -0.4256740239330940589, 0.5062356173688730143, 0.1616495878803643205 ) ) ;
#12405 = EDGE_CURVE ( 'NONE', #16795, #14218, #16041, .T. ) ;
#12406 = CARTESIAN_POINT ( 'NONE',  ( 0.3393484408203505942, 0.7678314947796125445, -0.7734693920224366970 ) ) ;
#12407 = CARTESIAN_POINT ( 'NONE',  ( 0.2521176338356569957, 0.2211428102655756955, 1.973425196850393970 ) ) ;
#12408 = ORIENTED_EDGE ( 'NONE', *, *, #22319, .F. ) ;
#12409 = ORIENTED_EDGE ( 'NONE', *, *, #4311, .T. ) ;
#12410 = CIRCLE ( 'NONE', #22318, 0.5007874015748031704 ) ;
#12411 = CARTESIAN_POINT ( 'NONE',  ( -0.4921259842519395411, 0.03220957031763951872, -1.550196850393700920 ) ) ;
#12412 = DIRECTION ( 'NONE',  ( 1.000000000000000000, 0.000000000000000000, 0.000000000000000000 ) ) ;
#12413 = CARTESIAN_POINT ( 'NONE',  ( -0.3714952424334504455, 0.06515381386493838967, 0.1992142436757342316 ) ) ;
#12414 = PRODUCT_RELATED_PRODUCT_CATEGORY ( 'part', '', ( #13189 ) ) ;
#12415 = AXIS2_PLACEMENT_3D ( 'NONE', #19850, #7001, #4589 ) ;
#12416 = ORIENTED_EDGE ( 'NONE', *, *, #15042, .T. ) ;
#12417 = ORIENTED_EDGE ( 'NONE', *, *, #22885, .F. ) ;
#12418 = ORIENTED_EDGE ( 'NONE', *, *, #11729, .T. ) ;
#12419 = EDGE_CURVE ( 'NONE', #1388, #15096, #15829, .T. ) ;
#12420 = EDGE_CURVE ( 'NONE', #27503, #5922, #110, .T. ) ;
#12421 = CARTESIAN_POINT ( 'NONE',  ( 0.0005056364805146920096, 0.3583524373837443933, 0.09506557084337925734 ) ) ;
#12422 = DIRECTION ( 'NONE',  ( 0.000000000000000000, 0.000000000000000000, -1.000000000000000000 ) ) ;
#12423 = DIRECTION ( 'NONE',  ( 0.000000000000000000, -1.000000000000000000, 0.000000000000000000 ) ) ;
#12424 = CIRCLE ( 'NONE', #19193, 0.8267716535433071723 ) ;
#12425 = ORIENTED_EDGE ( 'NONE', *, *, #24266, .T. ) ;
#12426 = DIRECTION ( 'NONE',  ( 1.000000000000000000, 0.000000000000000000, 0.000000000000000000 ) ) ;
#12427 = CARTESIAN_POINT ( 'NONE',  ( -0.3722026523000413478, 0.000000000000000000, -0.05511811023622047168 ) ) ;
#12428 = DIRECTION ( 'NONE',  ( 0.000000000000000000, 0.000000000000000000, 1.000000000000000000 ) ) ;
#12429 = CARTESIAN_POINT ( 'NONE',  ( 1.802543688615236173, 2.925196850393700920, 0.7677165354330708347 ) ) ;
#12430 = CARTESIAN_POINT ( 'NONE',  ( -0.4386012532733669644, -0.7958710277660615562, -0.03879670081233077550 ) ) ;
#12431 = AXIS2_PLACEMENT_3D ( 'NONE', #12868, #6519, #27721 ) ;
#12432 = DIRECTION ( 'NONE',  ( -1.000000000000000000, 0.000000000000000000, 0.000000000000000000 ) ) ;
#12433 = CARTESIAN_POINT ( 'NONE',  ( -0.5280876769851563513, 0.06947563356136872426, 1.747047244094487972 ) ) ;
#12434 = SHAPE_REPRESENTATION ( 'MAS-227', ( #16593, #22897, #14329, #21097, #10711, #2144, #4844, #25143, #20176, #12963, #11603, #8908, #16138, #787, #8019, #27411, #15248, #2584, #3012, #25617, #16524, #7557, #22853, #5253, #27823, #19298, #21052, #24197, #17441, #25161, #26018, #12485, #9347, #336, #8869, #22398, #24642, #2161, #744, #16098, #4428, #3911, #19705, #17912, #4365, #27982, #27995, #28008 ), #810 ) ;
#12435 = DIRECTION ( 'NONE',  ( 0.000000000000000000, 0.000000000000000000, -1.000000000000000000 ) ) ;
#12436 = EDGE_LOOP ( 'NONE', ( #23384, #1357, #11625, #18274 ) ) ;
#12437 = CARTESIAN_POINT ( 'NONE',  ( 0.4068940122748140875, 0.3122781343794410747, -1.550196850393701142 ) ) ;
#12438 = VERTEX_POINT ( 'NONE', #22674 ) ;
#12439 = SHAPE_REPRESENTATION_RELATIONSHIP ( 'NONE' , 'NONE' ,  #19852, #24825 ) ;
#12440 = CIRCLE ( 'NONE', #26842, 0.06200787401574803237 ) ;
#12441 = ORIENTED_EDGE ( 'NONE', *, *, #11215, .T. ) ;
#12442 = ORIENTED_EDGE ( 'NONE', *, *, #3958, .T. ) ;
#12443 = CARTESIAN_POINT ( 'NONE',  ( 0.5905511811023621549, 0.000000000000000000, -0.3740157480314960647 ) ) ;
#12444 = LINE ( 'NONE', #12021, #10759 ) ;
#12445 = CARTESIAN_POINT ( 'NONE',  ( 0.07214854559196579031, 0.5476281405333208729, 0.9202755905511811330 ) ) ;
#12446 = ORIENTED_EDGE ( 'NONE', *, *, #16486, .T. ) ;
#12447 = ADVANCED_FACE ( 'NONE', ( #9672 ), #11329, .F. ) ;
#12448 = DIRECTION ( 'NONE',  ( -1.000000000000000000, 0.000000000000000000, 0.000000000000000000 ) ) ;
#12449 = DIRECTION ( 'NONE',  ( 0.000000000000000000, 0.000000000000000000, -1.000000000000000000 ) ) ;
#12450 = EDGE_CURVE ( 'NONE', #13715, #24919, #19906, .T. ) ;
#12451 = AXIS2_PLACEMENT_3D ( 'NONE', #11432, #6662, #20052 ) ;
#12452 = CARTESIAN_POINT ( 'NONE',  ( 0.4537304931026562849, 0.07942646906837143306, 0.1771653543307087630 ) ) ;
#12453 = FACE_OUTER_BOUND ( 'NONE', #4969, .T. ) ;
#12454 = VECTOR ( 'NONE', #1903, 39.37007874015748143 ) ;
#12455 = CARTESIAN_POINT ( 'NONE',  ( -0.08600259748438122964, 0.2165354330708661457, -3.597797143241368456 ) ) ;
#12456 = ORIENTED_EDGE ( 'NONE', *, *, #6586, .T. ) ;
#12457 = CARTESIAN_POINT ( 'NONE',  ( 0.7874015748031151229, 0.2490421840548274757, -0.2751330019808225780 ) ) ;
#12458 = CARTESIAN_POINT ( 'NONE',  ( -0.04380447413658832695, 0.3324885138898346360, 1.953740157480315043 ) ) ;
#12459 = CARTESIAN_POINT ( 'NONE',  ( -0.5118110236220473341, 0.000000000000000000, -1.550196850393700920 ) ) ;
#12460 = EDGE_CURVE ( 'NONE', #12934, #12849, #2741, .T. ) ;
#12461 = DIRECTION ( 'NONE',  ( 0.000000000000000000, -1.000000000000000000, 0.000000000000000000 ) ) ;
#12462 = CARTESIAN_POINT ( 'NONE',  ( -0.3268939675028499914, -0.1881330340946393564, 0.1992125984251968684 ) ) ;
#12463 = DIRECTION ( 'NONE',  ( -0.9396926207859083169, -0.3420201433256692125, 0.000000000000000000 ) ) ;
#12464 = ORIENTED_EDGE ( 'NONE', *, *, #23719, .T. ) ;
#12465 = CARTESIAN_POINT ( 'NONE',  ( -0.3460530745557111598, 0.09275304139139804727, -3.115157480314960203 ) ) ;
#12466 = AXIS2_PLACEMENT_3D ( 'NONE', #24436, #19935, #590 ) ;
#12467 = ORIENTED_EDGE ( 'NONE', *, *, #7794, .T. ) ;
#12468 = ADVANCED_FACE ( 'NONE', ( #3301 ), #14044, .F. ) ;
#12469 = AXIS2_PLACEMENT_3D ( 'NONE', #4984, #7115, #14037 ) ;
#12470 = CARTESIAN_POINT ( 'NONE',  ( -0.5118110236220182463, 0.03349795313034509281, -1.550196850393700920 ) ) ;
#12471 = DIRECTION ( 'NONE',  ( 0.000000000000000000, 0.000000000000000000, 1.000000000000000000 ) ) ;
#12472 = DIRECTION ( 'NONE',  ( 0.000000000000000000, 0.000000000000000000, 1.000000000000000000 ) ) ;
#12473 = CARTESIAN_POINT ( 'NONE',  ( -0.6299212598425196763, -0.4526313213353582721, 0.9943460912301771426 ) ) ;
#12474 = ADVANCED_FACE ( 'NONE', ( #27059 ), #18534, .T. ) ;
#12475 = VERTEX_POINT ( 'NONE', #7711 ) ;
#12476 = CARTESIAN_POINT ( 'NONE',  ( -0.5622644009080379757, -0.5390998427249246161, 0.9826767787474022242 ) ) ;
#12477 = VERTEX_POINT ( 'NONE', #17983 ) ;
#12478 = DIRECTION ( 'NONE',  ( 0.000000000000000000, 1.000000000000000000, 0.000000000000000000 ) ) ;
#12479 = CARTESIAN_POINT ( 'NONE',  ( 0.000000000000000000, 0.000000000000000000, -4.370956692913385731E-17 ) ) ;
#12480 = CARTESIAN_POINT ( 'NONE',  ( 0.07874015748031495954, 0.1968503937007874127, -3.456364829396325167 ) ) ;
#12481 = CARTESIAN_POINT ( 'NONE',  ( 0.2315507648392299000, -0.4792806379917101678, 0.3401574803149606252 ) ) ;
#12482 = EDGE_CURVE ( 'NONE', #18347, #10433, #15894, .T. ) ;
#12483 = ORIENTED_EDGE ( 'NONE', *, *, #18476, .T. ) ;
#12484 = CARTESIAN_POINT ( 'NONE',  ( -0.2120693917185216271, -0.5839438448129662396, 0.2574819594177527593 ) ) ;
#12485 = AXIS2_PLACEMENT_3D ( 'NONE', #21469, #4093, #25280 ) ;
#12486 = LINE ( 'NONE', #4825, #8252 ) ;
#12487 = AXIS2_PLACEMENT_3D ( 'NONE', #5566, #26741, #7395 ) ;
#12488 = ORIENTED_EDGE ( 'NONE', *, *, #4655, .F. ) ;
#12489 = CARTESIAN_POINT ( 'NONE',  ( -0.3661417322834645272, 0.9448818897637796255, 0.1082677165354330451 ) ) ;
#12490 = CARTESIAN_POINT ( 'NONE',  ( 0.000000000000000000, 0.000000000000000000, 0.1771653543307086520 ) ) ;
#12492 = EDGE_CURVE ( 'NONE', #21046, #23841, #26479, .T. ) ;
#12491 = CARTESIAN_POINT ( 'NONE',  ( 0.2466292688015208900, -0.4270824798167630054, -1.569881889763779625 ) ) ;
#12493 = EDGE_CURVE ( 'NONE', #22690, #17082, #9980, .T. ) ;
#12494 = UNCERTAINTY_MEASURE_WITH_UNIT (LENGTH_MEASURE( 1.000000000000000082E-05 ), #904, 'distance_accuracy_value', 'NONE') ;
#12495 = CARTESIAN_POINT ( 'NONE',  ( 0.4527559054764770385, -0.02963280468032104126, -1.934055118110236338 ) ) ;
#12496 = CARTESIAN_POINT ( 'NONE',  ( 0.3979194638820598984, -0.2297883689023126064, -1.928289503579157183 ) ) ;
#12497 = VERTEX_POINT ( 'NONE', #21262 ) ;
#12498 = EDGE_LOOP ( 'NONE', ( #25731, #4495, #5923, #4131 ) ) ;
#12499 = VERTEX_POINT ( 'NONE', #1619 ) ;
#12500 = CARTESIAN_POINT ( 'NONE',  ( -0.6002615430280354714, -0.1993712550749956736, 0.2207846809961432899 ) ) ;
#12501 = CARTESIAN_POINT ( 'NONE',  ( 1.197070535079588716, 0.4724409448818898127, 1.078960298859116707 ) ) ;
#12502 = CARTESIAN_POINT ( 'NONE',  ( 0.4441657790107724213, -0.2564944395515492137, 1.747047244094488194 ) ) ;
#12503 = ORIENTED_EDGE ( 'NONE', *, *, #20952, .F. ) ;
#12504 = CARTESIAN_POINT ( 'NONE',  ( -0.3214446924536846772, 0.3840069416942866742, 0.09685039370078740717 ) ) ;
#12505 = ORIENTED_EDGE ( 'NONE', *, *, #8211, .F. ) ;
#12506 = CARTESIAN_POINT ( 'NONE',  ( -0.09842519685039370636, 0.2165354330708661457, -3.364501312335958172 ) ) ;
#12507 = CARTESIAN_POINT ( 'NONE',  ( 0.2169784220059887692, -0.4520537072416159208, 0.1643955689668546716 ) ) ;
#12508 = B_SPLINE_SURFACE_WITH_KNOTS ( 'NONE', 3, 3, ( 
 ( #2100, #15395, #27819, #23986 ),
 ( #8456, #17079, #6625, #25695 ),
 ( #10996, #4621, #19619, #15249 ),
 ( #8865, #2506, #12832, #34 ) ),
 .UNSPECIFIED., .F., .F., .F.,
 ( 4, 4 ),
 ( 4, 4 ),
 ( -0.3202300972144559998, -0.1691655120378159904 ),
 ( -4.440891999999999804E-16, 1.199999999999999956 ),
 .UNSPECIFIED. ) ;
#12509 = CARTESIAN_POINT ( 'NONE',  ( 0.2131049448084480213, -0.5835666837866708700, 0.2574803149606298969 ) ) ;
#12510 = EDGE_CURVE ( 'NONE', #3579, #4805, #14792, .T. ) ;
#12511 = CARTESIAN_POINT ( 'NONE',  ( 0.1141709026133643362, 0.3362336590883639453, 1.953740157480315043 ) ) ;
#12512 = ORIENTED_EDGE ( 'NONE', *, *, #14408, .T. ) ;
#12513 = FACE_OUTER_BOUND ( 'NONE', #6390, .T. ) ;
#12515 = CARTESIAN_POINT ( 'NONE',  ( -0.5708661417322835607, -0.03736310157554036115, 0.9399606299212598381 ) ) ;
#12514 = FACE_OUTER_BOUND ( 'NONE', #24150, .T. ) ;
#12516 = DIRECTION ( 'NONE',  ( 1.000000000000000000, 0.000000000000000000, 0.000000000000000000 ) ) ;
#12517 = DIRECTION ( 'NONE',  ( -1.000000000000000000, 0.000000000000000000, 0.000000000000000000 ) ) ;
#12518 = CYLINDRICAL_SURFACE ( 'NONE', #14014, 0.09679133858267717494 ) ;
#12519 = EDGE_CURVE ( 'NONE', #8591, #16564, #12216, .T. ) ;
#12520 = CARTESIAN_POINT ( 'NONE',  ( 0.02339816079119088829, 0.3574975638436101444, -3.115157480314960647 ) ) ;
#12521 = DIRECTION ( 'NONE',  ( 0.000000000000000000, 0.000000000000000000, 1.000000000000000000 ) ) ;
#12522 = CARTESIAN_POINT ( 'NONE',  ( 0.0001974756197918694275, 0.5007874015748031704, 0.2574827755769819038 ) ) ;
#12523 = DIRECTION ( 'NONE',  ( 0.000000000000000000, 0.000000000000000000, 1.000000000000000000 ) ) ;
#12524 = AXIS2_PLACEMENT_3D ( 'NONE', #2291, #10918, #4557 ) ;
#12525 = EDGE_CURVE ( 'NONE', #17898, #7118, #23153, .T. ) ;
#12526 = DIRECTION ( 'NONE',  ( 0.000000000000000000, 0.000000000000000000, -1.000000000000000000 ) ) ;
#12527 = CARTESIAN_POINT ( 'NONE',  ( 1.857656692913385893E-16, 0.000000000000000000, 0.000000000000000000 ) ) ;
#12528 = VECTOR ( 'NONE', #6452, 39.37007874015748143 ) ;
#12529 = ORIENTED_EDGE ( 'NONE', *, *, #18189, .T. ) ;
#12530 = CARTESIAN_POINT ( 'NONE',  ( 0.003937007874015826907, -4.393043307086613241E-18, 0.000000000000000000 ) ) ;
#12531 = COLOUR_RGB ( '', 0.09019608, 0.27058824, 0.51372549) ;
#12532 = CARTESIAN_POINT ( 'NONE',  ( 0.000000000000000000, 0.000000000000000000, 0.1377952755905511861 ) ) ;
#12533 = ORIENTED_EDGE ( 'NONE', *, *, #21382, .F. ) ;
#12534 = EDGE_LOOP ( 'NONE', ( #21978, #25205 ) ) ;
#12535 = MANIFOLD_SOLID_BREP ( 'O-Ring 26.5x2.65', #622 ) ;
#12536 = EDGE_LOOP ( 'NONE', ( #26095, #15084 ) ) ;
#12537 = DIRECTION ( 'NONE',  ( 0.000000000000000000, -1.000000000000000000, 0.000000000000000000 ) ) ;
#12538 = CARTESIAN_POINT ( 'NONE',  ( 0.5043504886477717664, -0.1712563538833085097, 1.747047244094488194 ) ) ;
#12539 = CARTESIAN_POINT ( 'NONE',  ( -0.3015072509068622009, 0.3596217111731054850, 0.07637549214372835182 ) ) ;
#12540 = CARTESIAN_POINT ( 'NONE',  ( 0.1493967478962656692, -0.4798749592428788180, -0.01883130896440190702 ) ) ;
#12541 = EDGE_LOOP ( 'NONE', ( #18549, #26598, #10131, #2098, #4414 ) ) ;
#12542 = ORIENTED_EDGE ( 'NONE', *, *, #7577, .T. ) ;
#12543 = CARTESIAN_POINT ( 'NONE',  ( 0.3551931031211519874, -0.04679574315772458415, -3.115157480314960647 ) ) ;
#12544 = VERTEX_POINT ( 'NONE', #4027 ) ;
#12545 = CARTESIAN_POINT ( 'NONE',  ( -0.4585215200179055817, 2.807634559150536355E-17, -1.928289503579156516 ) ) ;
#12546 = DIRECTION ( 'NONE',  ( 0.3174974722037089969, 3.888222630716479561E-17, -0.9482591181445370054 ) ) ;
#12547 = EDGE_CURVE ( 'NONE', #1638, #17537, #1864, .T. ) ;
#12548 = AXIS2_PLACEMENT_3D ( 'NONE', #4790, #13281, #21905 ) ;
#12549 = CARTESIAN_POINT ( 'NONE',  ( -0.04380447413658627998, 0.3324885138898243664, 1.973425196850393970 ) ) ;
#12550 = ORIENTED_EDGE ( 'NONE', *, *, #556, .T. ) ;
#12551 = ORIENTED_EDGE ( 'NONE', *, *, #211, .F. ) ;
#12552 = CARTESIAN_POINT ( 'NONE',  ( 0.03220957031753989008, 0.4921259842519685179, -1.550196850393700920 ) ) ;
#12553 = CIRCLE ( 'NONE', #1774, 0.6881889763779527325 ) ;
#12554 = FACE_BOUND ( 'NONE', #7951, .T. ) ;
#12555 = AXIS2_PLACEMENT_3D ( 'NONE', #11925, #9365, #20116 ) ;
#12556 = ORIENTED_EDGE ( 'NONE', *, *, #18908, .T. ) ;
#12557 = ORIENTED_EDGE ( 'NONE', *, *, #19567, .F. ) ;
#12558 = ORIENTED_EDGE ( 'NONE', *, *, #25273, .T. ) ;
#12559 = DIRECTION ( 'NONE',  ( 0.000000000000000000, 0.000000000000000000, -1.000000000000000000 ) ) ;
#12560 = CARTESIAN_POINT ( 'NONE',  ( -0.2421724791772047192, 0.2891474103999575052, 0.1992142436757342316 ) ) ;
#12561 = AXIS2_PLACEMENT_3D ( 'NONE', #7214, #15832, #24308 ) ;
#12562 = CYLINDRICAL_SURFACE ( 'NONE', #9651, 0.3937007874015748254 ) ;
#12563 = ORIENTED_EDGE ( 'NONE', *, *, #26186, .F. ) ;
#12564 = VERTEX_POINT ( 'NONE', #12501 ) ;
#12565 = CARTESIAN_POINT ( 'NONE',  ( -0.2362204724409449064, 0.000000000000000000, 0.000000000000000000 ) ) ;
#12566 = FACE_OUTER_BOUND ( 'NONE', #16555, .T. ) ;
#12567 = EDGE_CURVE ( 'NONE', #11990, #18223, #21732, .T. ) ;
#12568 = DIRECTION ( 'NONE',  ( -1.000000000000000000, 0.000000000000000000, 0.000000000000000000 ) ) ;
#12569 = TOROIDAL_SURFACE ( 'NONE', #8062, 0.3740157480314960647, 0.03937007874015747977 ) ;
#12570 = DIRECTION ( 'NONE',  ( -1.000000000000000000, 0.000000000000000000, 0.000000000000000000 ) ) ;
#12571 = AXIS2_PLACEMENT_3D ( 'NONE', #4685, #471, #8658 ) ;
#12572 = CYLINDRICAL_SURFACE ( 'NONE', #8766, 0.1673228346456692994 ) ;
#12573 = LINE ( 'NONE', #25845, #12842 ) ;
#12574 = DIRECTION ( 'NONE',  ( 0.000000000000000000, 0.000000000000000000, -1.000000000000000000 ) ) ;
#12575 = VERTEX_POINT ( 'NONE', #21116 ) ;
#12576 = EDGE_CURVE ( 'NONE', #8924, #26710, #5471, .T. ) ;
#12577 = AXIS2_PLACEMENT_3D ( 'NONE', #21344, #1979, #10741 ) ;
#12578 = ORIENTED_EDGE ( 'NONE', *, *, #2388, .T. ) ;
#12579 = CARTESIAN_POINT ( 'NONE',  ( 0.2992781133269515892, -0.6197069291944330427, 0.3401574803149606252 ) ) ;
#12580 = ORIENTED_EDGE ( 'NONE', *, *, #22683, .T. ) ;
#12581 = CYLINDRICAL_SURFACE ( 'NONE', #11112, 0.7283464566929134243 ) ;
#12582 = CARTESIAN_POINT ( 'NONE',  ( 0.6299212598425196763, 7.714310545810098438E-17, -4.370956692913385731E-17 ) ) ;
#12583 = CARTESIAN_POINT ( 'NONE',  ( -0.1429116519061127688, 0.5335524835332354776, 0.9202755905511811330 ) ) ;
#12584 = ORIENTED_EDGE ( 'NONE', *, *, #13683, .T. ) ;
#12585 = CARTESIAN_POINT ( 'NONE',  ( 0.000000000000000000, 0.000000000000000000, 2.504921259842519898 ) ) ;
#12586 = ORIENTED_EDGE ( 'NONE', *, *, #6335, .F. ) ;
#12587 = CIRCLE ( 'NONE', #23892, 0.6889763779527560139 ) ;
#12588 = LINE ( 'NONE', #10039, #20825 ) ;
#12589 = AXIS2_PLACEMENT_3D ( 'NONE', #2240, #23872, #3050 ) ;
#12590 = AXIS2_PLACEMENT_3D ( 'NONE', #9073, #8430, #24198 ) ;
#12591 = CARTESIAN_POINT ( 'NONE',  ( 0.000000000000000000, -1.533249767903113305E-16, -0.3163739521363750362 ) ) ;
#12592 = ADVANCED_FACE ( 'NONE', ( #9953 ), #15843, .F. ) ;
#12593 = PLANE ( 'NONE',  #27676 ) ;
#12594 = ORIENTED_EDGE ( 'NONE', *, *, #14264, .F. ) ;
#12595 = CARTESIAN_POINT ( 'NONE',  ( -0.3661417322834645272, 0.9448818897637796255, -1.639108661417322569E-17 ) ) ;
#12596 = VERTEX_POINT ( 'NONE', #1480 ) ;
#12597 = TOROIDAL_SURFACE ( 'NONE', #883, 0.6102362204724409711, 0.1299212598425196763 ) ;
#12598 = CARTESIAN_POINT ( 'NONE',  ( -0.08676778863011123943, 0.3239425792934299553, 1.953740157480315043 ) ) ;
#12599 = LINE ( 'NONE', #12871, #7606 ) ;
#12600 = ADVANCED_FACE ( 'NONE', ( #22964 ), #13148, .T. ) ;
#12601 = CARTESIAN_POINT ( 'NONE',  ( 0.02916473398703041744, -0.07408303521633090305, -0.4653527282821430799 ) ) ;
#12602 = CARTESIAN_POINT ( 'NONE',  ( 0.03607471876262466348, 0.5511811023622048555, 0.9399606299212598381 ) ) ;
#12603 = CARTESIAN_POINT ( 'NONE',  ( 0.2427018018350767803, 0.2887032559529629783, 0.1992142436757342316 ) ) ;
#12604 = CARTESIAN_POINT ( 'NONE',  ( -1.197070535079588716, 0.4724409448818898127, -1.315180771300060503 ) ) ;
#12605 = EDGE_LOOP ( 'NONE', ( #5775, #5595, #18988, #19242, #2611, #19985 ) ) ;
#12606 = CARTESIAN_POINT ( 'NONE',  ( 0.2361997806693254542, 0.2693761163850786344, -3.115157480314960647 ) ) ;
#12607 = EDGE_CURVE ( 'NONE', #11359, #9393, #14059, .T. ) ;
#12608 = CIRCLE ( 'NONE', #19816, 0.4803149606299212393 ) ;
#12609 = CARTESIAN_POINT ( 'NONE',  ( 0.000000000000000000, 0.000000000000000000, 0.2362204724409449064 ) ) ;
#12610 = CONICAL_SURFACE ( 'NONE', #5382, 0.1106489370078740930, 0.08726646250000029414 ) ;
#12611 = ADVANCED_FACE ( 'NONE', ( #6165 ), #10007, .F. ) ;
#12612 = AXIS2_PLACEMENT_3D ( 'NONE', #12867, #13287, #17388 ) ;
#12613 = ORIENTED_EDGE ( 'NONE', *, *, #12244, .F. ) ;
#12614 = CARTESIAN_POINT ( 'NONE',  ( -0.03746919241598681977, -0.5708647227724242823, 0.9399606299212600602 ) ) ;
#12615 = CARTESIAN_POINT ( 'NONE',  ( -1.928513779527558736E-17, 0.000000000000000000, -0.03543307086614204404 ) ) ;
#12616 = CARTESIAN_POINT ( 'NONE',  ( -2.073220866141732523E-16, 0.4724409448818898127, 1.574803149606299524 ) ) ;
#12617 = CARTESIAN_POINT ( 'NONE',  ( -0.3242892624568586291, -0.4225434286519560989, 1.747047244094488194 ) ) ;
#12618 = CARTESIAN_POINT ( 'NONE',  ( 0.1327952259511945843, 0.4954219348936774736, -1.550196850393700476 ) ) ;
#12619 = CARTESIAN_POINT ( 'NONE',  ( -0.5776040203856925848, -0.4807978361611910945, 0.9954634121921446255 ) ) ;
#12620 = VERTEX_POINT ( 'NONE', #23670 ) ;
#12621 = CARTESIAN_POINT ( 'NONE',  ( -0.6020310366335483998, -0.5839878592438488836, -0.9562163583985735515 ) ) ;
#12622 = DIRECTION ( 'NONE',  ( 0.000000000000000000, -1.000000000000000000, 0.000000000000000000 ) ) ;
#12623 = CARTESIAN_POINT ( 'NONE',  ( -0.7874015748031496509, 0.4828108945773819105, 0.1423708153504031348 ) ) ;
#12624 = LINE ( 'NONE', #1885, #1423 ) ;
#12625 = ORIENTED_EDGE ( 'NONE', *, *, #19218, .F. ) ;
#12626 = TOROIDAL_SURFACE ( 'NONE', #457, 0.5393700787401575214, 0.01181102362204724393 ) ;
#12627 = DIRECTION ( 'NONE',  ( -1.000000000000000000, 0.000000000000000000, 0.000000000000000000 ) ) ;
#12628 = CIRCLE ( 'NONE', #3122, 0.3163739521363750362 ) ;
#12629 = CARTESIAN_POINT ( 'NONE',  ( 0.1504127680534947942, 0.4837205684772488690, 0.03783905811611818631 ) ) ;
#12630 = ORIENTED_EDGE ( 'NONE', *, *, #10822, .T. ) ;
#12631 = CARTESIAN_POINT ( 'NONE',  ( 0.2761764805255614297, 0.3599896729929412120, -1.934055118110236338 ) ) ;
#12632 = EDGE_CURVE ( 'NONE', #22435, #5635, #26318, .T. ) ;
#12633 = DIRECTION ( 'NONE',  ( 0.000000000000000000, 0.000000000000000000, -1.000000000000000000 ) ) ;
#12634 = EDGE_CURVE ( 'NONE', #19774, #24768, #11349, .T. ) ;
#12635 = VERTEX_POINT ( 'NONE', #13056 ) ;
#12636 = CARTESIAN_POINT ( 'NONE',  ( -0.5355664161054535244, -0.3771716564148893669, 0.01418171057387437005 ) ) ;
#12637 = CARTESIAN_POINT ( 'NONE',  ( 0.000000000000000000, 0.000000000000000000, 39.92337183164450920 ) ) ;
#12638 = CARTESIAN_POINT ( 'NONE',  ( -0.3122922550266335473, 0.3730863453124460549, 0.1075369453635828670 ) ) ;
#12639 = AXIS2_PLACEMENT_3D ( 'NONE', #6825, #21939, #13311 ) ;
#12640 = ORIENTED_EDGE ( 'NONE', *, *, #18523, .T. ) ;
#12641 = CIRCLE ( 'NONE', #24348, 0.09679133858267717494 ) ;
#12642 = CARTESIAN_POINT ( 'NONE',  ( -0.07874015748031495954, 0.04546065111729338803, -0.4724409448818898127 ) ) ;
#12643 = CARTESIAN_POINT ( 'NONE',  ( -0.6138529921540000212, -0.4891471943186955773, 0.9948696824541676254 ) ) ;
#12644 = DIRECTION ( 'NONE',  ( 0.000000000000000000, -1.000000000000000000, 0.000000000000000000 ) ) ;
#12645 = CARTESIAN_POINT ( 'NONE',  ( 0.1120675189988346587, -0.7410715175625038897, 0.001857066358701141805 ) ) ;
#12646 = CARTESIAN_POINT ( 'NONE',  ( 0.04638120790932724613, 0.3520466617656882735, 1.953740157480315043 ) ) ;
#12647 = EDGE_CURVE ( 'NONE', #16194, #2567, #4144, .T. ) ;
#12648 = CIRCLE ( 'NONE', #936, 0.6299212598425196763 ) ;
#12649 = CARTESIAN_POINT ( 'NONE',  ( -0.6104814441609700548, -0.1036450511418069570, -0.2428261403048069811 ) ) ;
#12650 = CARTESIAN_POINT ( 'NONE',  ( 0.4063220079890716430, -0.2348123150948751847, 0.1992150590373740204 ) ) ;
#12651 = VERTEX_POINT ( 'NONE', #12773 ) ;
#12652 = EDGE_LOOP ( 'NONE', ( #8229, #2480, #27410, #14347 ) ) ;
#12653 = DIRECTION ( 'NONE',  ( 0.000000000000000000, 1.000000000000000000, 0.000000000000000000 ) ) ;
#12654 = DIRECTION ( 'NONE',  ( -1.000000000000000000, 0.000000000000000000, 0.000000000000000000 ) ) ;
#12655 = CARTESIAN_POINT ( 'NONE',  ( 0.2272836761397900307, -0.2962590301041579388, -3.115157480314960647 ) ) ;
#12656 = DIRECTION ( 'NONE',  ( 1.000000000000000000, 0.000000000000000000, 0.000000000000000000 ) ) ;
#12657 = DIRECTION ( 'NONE',  ( -1.000000000000000000, 0.000000000000000000, 0.000000000000000000 ) ) ;
#12658 = CARTESIAN_POINT ( 'NONE',  ( -0.5511811023622047445, 0.000000000000000000, 0.000000000000000000 ) ) ;
#12659 = CARTESIAN_POINT ( 'NONE',  ( -0.1968503937007874127, 0.9448818897637796255, -1.639108661417322569E-17 ) ) ;
#12660 = CARTESIAN_POINT ( 'NONE',  ( 0.4921259842519685179, 2.987958743070287587E-17, -1.569881889763779625 ) ) ;
#12661 = CIRCLE ( 'NONE', #18026, 0.1299232283464567261 ) ;
#12662 = ADVANCED_FACE ( 'NONE', ( #6982, #6705 ), #13329, .T. ) ;
#12663 = EDGE_CURVE ( 'NONE', #8364, #9929, #2306, .T. ) ;
#12664 = VERTEX_POINT ( 'NONE', #21399 ) ;
#12665 = CARTESIAN_POINT ( 'NONE',  ( -0.1838434515542552161, 0.5417490723636845251, 0.9399606299212600602 ) ) ;
#12666 = MANIFOLD_SOLID_BREP ( 'Cam Follower', #17746 ) ;
#12667 = VERTEX_POINT ( 'NONE', #365 ) ;
#12668 = CARTESIAN_POINT ( 'NONE',  ( -0.4359497604187455577, 0.2332958656722624868, -0.2680411597722005546 ) ) ;
#12669 = CARTESIAN_POINT ( 'NONE',  ( 0.5869493968219645641, 0.2133897621573074832, 0.3696019098714952711 ) ) ;
#12670 = APPLICATION_PROTOCOL_DEFINITION ( 'draft international standard', 'automotive_design', 1998, #4568 ) ;
#12671 = DIMENSIONAL_EXPONENTS ( 1.000000000000000000, 0.000000000000000000, 0.000000000000000000, 0.000000000000000000, 0.000000000000000000, 0.000000000000000000, 0.000000000000000000 ) ;
#12672 = DIRECTION ( 'NONE',  ( 0.000000000000000000, -1.000000000000000000, 0.000000000000000000 ) ) ;
#12673 = ADVANCED_FACE ( 'NONE', ( #4570 ), #10797, .T. ) ;
#12674 = ORIENTED_EDGE ( 'NONE', *, *, #21441, .F. ) ;
#12675 = ORIENTED_EDGE ( 'NONE', *, *, #5, .F. ) ;
#12676 = CARTESIAN_POINT ( 'NONE',  ( -0.1791601451668923262, -0.3102476824511486986, -3.115157480314960647 ) ) ;
#12677 = CARTESIAN_POINT ( 'NONE',  ( -0.3666644560843326794, -0.2817828961649162522, -1.928289503579156516 ) ) ;
#12678 = CARTESIAN_POINT ( 'NONE',  ( -0.2982299571022201667, 0.3545282230887890074, 0.2048502514545687270 ) ) ;
#12679 = CARTESIAN_POINT ( 'NONE',  ( -0.1677079028045458664, 0.2904160862623615391, 1.973425196850393970 ) ) ;
#12680 = EDGE_CURVE ( 'NONE', #27484, #15505, #19479, .T. ) ;
#12681 = ORIENTED_EDGE ( 'NONE', *, *, #6802, .F. ) ;
#12682 = ORIENTED_EDGE ( 'NONE', *, *, #25296, .F. ) ;
#12683 = AXIS2_PLACEMENT_3D ( 'NONE', #8960, #15877, #17709 ) ;
#12684 = DIRECTION ( 'NONE',  ( 1.000000000000000000, 0.000000000000000000, 0.000000000000000000 ) ) ;
#12685 = VERTEX_POINT ( 'NONE', #6842 ) ;
#12686 = EDGE_LOOP ( 'NONE', ( #10168, #16375, #6960, #21128 ) ) ;
#12687 = CARTESIAN_POINT ( 'NONE',  ( -0.2490711204941346568, 0.7655264129003995777, -0.7689379837741201484 ) ) ;
#12688 = CIRCLE ( 'NONE', #13147, 0.4606299212598425341 ) ;
#12689 = DIRECTION ( 'NONE',  ( 1.000000000000000000, 0.000000000000000000, 0.000000000000000000 ) ) ;
#12690 = CARTESIAN_POINT ( 'NONE',  ( -0.07874642858611770324, 0.3051016904613214620, -3.608673911198624129 ) ) ;
#12691 = VERTEX_POINT ( 'NONE', #15188 ) ;
#12692 = EDGE_CURVE ( 'NONE', #11355, #9025, #19038, .T. ) ;
#12693 = CARTESIAN_POINT ( 'NONE',  ( 0.3020416211906299941, -0.1738080303477508304, 0.1589462317999085772 ) ) ;
#12694 = ( REPRESENTATION_RELATIONSHIP ('NONE','NONE', #12434, #16232 ) REPRESENTATION_RELATIONSHIP_WITH_TRANSFORMATION ( #1818 )SHAPE_REPRESENTATION_RELATIONSHIP( ) ) ;
#12695 = ADVANCED_FACE ( 'NONE', ( #237 ), #24067, .T. ) ;
#12696 = DIRECTION ( 'NONE',  ( 0.000000000000000000, 0.000000000000000000, 1.000000000000000000 ) ) ;
#12697 = DIRECTION ( 'NONE',  ( 0.000000000000000000, 0.000000000000000000, 1.000000000000000000 ) ) ;
#12698 = EDGE_CURVE ( 'NONE', #16453, #720, #5115, .T. ) ;
#12699 = TOROIDAL_SURFACE ( 'NONE', #8646, 0.4055118110236220486, 0.01181102362204724393 ) ;
#12700 = CARTESIAN_POINT ( 'NONE',  ( -0.5942349471504173586, -0.2203927747844337814, 0.2172369878168960988 ) ) ;
#12701 = CARTESIAN_POINT ( 'NONE',  ( -0.4585215200179055817, 2.807634559150536355E-17, -1.928289503579156516 ) ) ;
#12702 = FACE_OUTER_BOUND ( 'NONE', #15120, .T. ) ;
#12703 = DIRECTION ( 'NONE',  ( 0.000000000000000000, -1.000000000000000000, 0.000000000000000000 ) ) ;
#12704 = VECTOR ( 'NONE', #6512, 39.37007874015748143 ) ;
#12705 = CARTESIAN_POINT ( 'NONE',  ( -0.02061007003135897908, 0.1968503937007873850, -3.195947033497543721 ) ) ;
#12706 = CARTESIAN_POINT ( 'NONE',  ( 0.000000000000000000, 0.000000000000000000, 0.02362204724409448786 ) ) ;
#12707 = VERTEX_POINT ( 'NONE', #22641 ) ;
#12708 = DIRECTION ( 'NONE',  ( 0.000000000000000000, 0.000000000000000000, -1.000000000000000000 ) ) ;
#12709 = ORIENTED_EDGE ( 'NONE', *, *, #12347, .F. ) ;
#12710 = DIRECTION ( 'NONE',  ( -0.2036417511401763802, 0.4895227362422922557, 0.8478782506317883438 ) ) ;
#12711 = MANIFOLD_SOLID_BREP ( 'Cam Shaft', #2849 ) ;
#12712 = CARTESIAN_POINT ( 'NONE',  ( 0.0007882571242861507056, 0.7401570605739641318, 0.2562996995998030880 ) ) ;
#12713 = CARTESIAN_POINT ( 'NONE',  ( -0.009795313329541911057, -0.08526597544697904485, -0.4724409448818898127 ) ) ;
#12714 = VERTEX_POINT ( 'NONE', #20383 ) ;
#12715 = DIRECTION ( 'NONE',  ( 0.000000000000000000, 0.000000000000000000, -1.000000000000000000 ) ) ;
#12716 = VERTEX_POINT ( 'NONE', #900 ) ;
#12717 = ADVANCED_FACE ( 'NONE', ( #3130, #9487 ), #5412, .T. ) ;
#12718 = CARTESIAN_POINT ( 'NONE',  ( 0.3268939675028499914, -0.1881330340946397728, 0.07637795275590551769 ) ) ;
#12719 = FILL_AREA_STYLE ('',( #9030 ) ) ;
#12720 = CIRCLE ( 'NONE', #18081, 0.1771653543307086798 ) ;
#12721 = CARTESIAN_POINT ( 'NONE',  ( -0.4690668203718997287, 0.08212126673591825521, 0.2330651857806316507 ) ) ;
#12722 = LINE ( 'NONE', #2398, #22639 ) ;
#12723 = CARTESIAN_POINT ( 'NONE',  ( -0.6711032387266614441, -0.1523958994813200962, 0.1322834645669291320 ) ) ;
#12724 = B_SPLINE_CURVE_WITH_KNOTS ( 'NONE', 3,
 ( #9284, #2661, #26669, #11017, #5058, #17510, #26129, #7187, #15806, #4645 ),
 .UNSPECIFIED., .F., .F.,
 ( 4, 2, 2, 2, 4 ),
 ( 0.000000000000000000, 0.2500000000000000000, 0.5000000000000000000, 0.7500000000000000000, 1.000000000000000000 ),
 .UNSPECIFIED. ) ;
#12725 = CIRCLE ( 'NONE', #153, 0.8267716535433071723 ) ;
#12726 = ORIENTED_EDGE ( 'NONE', *, *, #12146, .F. ) ;
#12727 = LINE ( 'NONE', #12200, #5318 ) ;
#12728 = CARTESIAN_POINT ( 'NONE',  ( 0.2299571666357553834, 0.2748389102014165974, 0.1805249803392612040 ) ) ;
#12729 = EDGE_CURVE ( 'NONE', #13999, #8723, #9539, .T. ) ;
#12730 = ORIENTED_EDGE ( 'NONE', *, *, #20207, .F. ) ;
#12731 = LINE ( 'NONE', #21639, #17931 ) ;
#12732 = FACE_OUTER_BOUND ( 'NONE', #1801, .T. ) ;
#12733 = CARTESIAN_POINT ( 'NONE',  ( 0.4173228346456693272, 0.000000000000000000, 0.4724409448818898127 ) ) ;
#12734 = CARTESIAN_POINT ( 'NONE',  ( 0.5476281405333119912, 0.07214854559198101425, 0.9399606299212598381 ) ) ;
#12735 = CARTESIAN_POINT ( 'NONE',  ( -0.09139240964747703810, 0.07874015748031500117, 0.02109836160874967170 ) ) ;
#12736 = EDGE_LOOP ( 'NONE', ( #320, #789 ) ) ;
#12737 = PRODUCT_DEFINITION_SHAPE ( 'NONE', 'NONE',  #22417 ) ;
#12738 = CARTESIAN_POINT ( 'NONE',  ( -0.2693761163850975637, 0.2361997806693252044, -3.115157480314961091 ) ) ;
#12739 = CIRCLE ( 'NONE', #16352, 0.5322834645669292097 ) ;
#12740 = VECTOR ( 'NONE', #19778, 39.37007874015748854 ) ;
#12741 = ORIENTED_EDGE ( 'NONE', *, *, #2389, .T. ) ;
#12742 = AXIS2_PLACEMENT_3D ( 'NONE', #5003, #13624, #20266 ) ;
#12743 = CARTESIAN_POINT ( 'NONE',  ( -0.1327036767636164405, 0.4954415918535620134, -1.550196850393700920 ) ) ;
#12744 = ORIENTED_EDGE ( 'NONE', *, *, #8516, .F. ) ;
#12745 = CARTESIAN_POINT ( 'NONE',  ( -0.5417490723642327533, -0.1838434515534312919, 0.9399606299212597271 ) ) ;
#12746 = LINE ( 'NONE', #17545, #23758 ) ;
#12747 = CARTESIAN_POINT ( 'NONE',  ( 0.4681308612729634389, -0.1074986424507603650, 0.2194422276442969111 ) ) ;
#12748 = DIRECTION ( 'NONE',  ( 0.000000000000000000, 0.000000000000000000, 1.000000000000000000 ) ) ;
#12749 = EDGE_CURVE ( 'NONE', #5588, #20420, #11617, .T. ) ;
#12750 = CARTESIAN_POINT ( 'NONE',  ( 0.2268956277329844951, 0.4599954779395432625, -1.550196850393701364 ) ) ;
#12751 = DIRECTION ( 'NONE',  ( -0.000000000000000000, 1.000000000000000000, -0.000000000000000000 ) ) ;
#12752 = ORIENTED_EDGE ( 'NONE', *, *, #14669, .F. ) ;
#12753 = ORIENTED_EDGE ( 'NONE', *, *, #18277, .T. ) ;
#12754 = EDGE_CURVE ( 'NONE', #21440, #11663, #536, .T. ) ;
#12755 = CARTESIAN_POINT ( 'NONE',  ( 0.2223167940359795647, 0.2657206863494898097, 0.1276989850598370946 ) ) ;
#12756 = DIRECTION ( 'NONE',  ( 0.000000000000000000, 0.000000000000000000, 1.000000000000000000 ) ) ;
#12757 = CARTESIAN_POINT ( 'NONE',  ( 0.4133615125891543784, 0.4936731914948853661, 0.2359405056213505492 ) ) ;
#12758 = PLANE ( 'NONE',  #17225 ) ;
#12759 = EDGE_CURVE ( 'NONE', #13503, #1758, #24429, .T. ) ;
#12760 = EDGE_LOOP ( 'NONE', ( #1232, #21202 ) ) ;
#12761 = CARTESIAN_POINT ( 'NONE',  ( 0.000000000000000000, 0.000000000000000000, 2.090519358671640647E-11 ) ) ;
#12762 = AXIS2_PLACEMENT_3D ( 'NONE', #13761, #3151, #18105 ) ;
#12763 = DIRECTION ( 'NONE',  ( 1.000000000000000000, 0.000000000000000000, 0.000000000000000000 ) ) ;
#12764 = CARTESIAN_POINT ( 'NONE',  ( -0.2146455952193271344, -0.4472013107423940537, 0.1734435147757991957 ) ) ;
#12765 = EDGE_CURVE ( 'NONE', #21578, #15239, #132, .T. ) ;
#12766 = EDGE_CURVE ( 'NONE', #10805, #1064, #4981, .T. ) ;
#12767 = ORIENTED_EDGE ( 'NONE', *, *, #14872, .F. ) ;
#12768 = CARTESIAN_POINT ( 'NONE',  ( 0.3599896729929407679, 0.2761764805255620403, -1.934055118110236338 ) ) ;
#12769 = DIRECTION ( 'NONE',  ( -0.9790454724845842893, 0.2036417511401760472, 0.000000000000000000 ) ) ;
#12770 = VERTEX_POINT ( 'NONE', #20098 ) ;
#12771 = EDGE_LOOP ( 'NONE', ( #18940, #6070, #17357, #8322 ) ) ;
#12772 = CARTESIAN_POINT ( 'NONE',  ( -0.4995226175161708859, -0.4253379528844141721, -0.1763862759506159561 ) ) ;
#12773 = CARTESIAN_POINT ( 'NONE',  ( 0.4247824284860164945, -5.202084413794395869E-17, -0.04133858267716535029 ) ) ;
#12774 = CARTESIAN_POINT ( 'NONE',  ( 0.4612490782034816550, -0.2663596103035388296, 1.747047244094488194 ) ) ;
#12775 = FACE_OUTER_BOUND ( 'NONE', #2580, .T. ) ;
#12776 = FACE_OUTER_BOUND ( 'NONE', #27394, .T. ) ;
#12777 = AXIS2_PLACEMENT_3D ( 'NONE', #16227, #9858, #18458 ) ;
#12778 = CARTESIAN_POINT ( 'NONE',  ( 0.4009292313364363758, -0.2321359940641732067, 0.2048502514564785326 ) ) ;
#12779 = AXIS2_PLACEMENT_3D ( 'NONE', #6331, #25256, #14963 ) ;
#12780 = CARTESIAN_POINT ( 'NONE',  ( -0.3534635626044764778, 0.2712695779735687651, -1.934055118110236116 ) ) ;
#12781 = ORIENTED_EDGE ( 'NONE', *, *, #23168, .T. ) ;
#12782 = CARTESIAN_POINT ( 'NONE',  ( -0.1570220809524502104, -0.3184841198566448206, 1.953740157480315043 ) ) ;
#12783 = EDGE_LOOP ( 'NONE', ( #23832, #25360, #3589, #15186 ) ) ;
#12784 = ORIENTED_EDGE ( 'NONE', *, *, #21668, .T. ) ;
#12785 = ADVANCED_FACE ( 'NONE', ( #9342 ), #17952, .F. ) ;
#12786 = EDGE_CURVE ( 'NONE', #18597, #12499, #14576, .T. ) ;
#12787 = TOROIDAL_SURFACE ( 'NONE', #7811, 0.5610236220472440971, 0.1003937007874015908 ) ;
#12788 = LINE ( 'NONE', #10104, #7165 ) ;
#12789 = CARTESIAN_POINT ( 'NONE',  ( -0.5692936381918457522, -0.3294684677439395637, 0.2081850588301124849 ) ) ;
#12790 = CARTESIAN_POINT ( 'NONE',  ( 0.2529800193559499921, -0.5131133041954075713, 0.9399606299212598381 ) ) ;
#12791 = CIRCLE ( 'NONE', #27685, 0.1318897637674583401 ) ;
#12792 = CARTESIAN_POINT ( 'NONE',  ( 0.1518453844022533417, -0.2938239883722331136, -0.3972446186644590371 ) ) ;
#12793 = CARTESIAN_POINT ( 'NONE',  ( 0.4173228346456693272, 0.000000000000000000, 0.02362204724409448786 ) ) ;
#12794 = LINE ( 'NONE', #21420, #20345 ) ;
#12795 = EDGE_CURVE ( 'NONE', #10563, #25079, #15010, .T. ) ;
#12796 = CARTESIAN_POINT ( 'NONE',  ( 0.3702005978258383068, -0.04877294052296102245, -3.115157480314960647 ) ) ;
#12797 = EDGE_CURVE ( 'NONE', #12849, #27168, #23184, .T. ) ;
#12798 = CARTESIAN_POINT ( 'NONE',  ( 0.5981657849660177995, 0.000000000000000000, 0.000000000000000000 ) ) ;
#12799 = DIRECTION ( 'NONE',  ( 0.000000000000000000, 1.000000000000000000, 0.000000000000000000 ) ) ;
#12800 = FACE_OUTER_BOUND ( 'NONE', #24975, .T. ) ;
#12801 = CLOSED_SHELL ( 'NONE', ( #9180, #580, #3832, #17393, #4276, #17492, #21556, #16210, #27630, #10037, #300, #21214, #20500, #23651, #26828, #19163, #5681, #18345, #19845, #7631, #27378, #8314, #1285, #1784, #8141, #17048, #13753, #15611, #16856, #13032, #17129, #27324, #22010, #27462, #16373, #10488, #13645, #4920, #4749, #3957, #26907, #63, #26730, #11974, #10926, #26307, #7263, #1026, #6579, #7222, #3576, #14335, #16992, #23014, #2675, #15242, #5581, #7446, #344, #12717, #19871, #1594, #16626, #25631, #4223, #10939, #595, #10363, #24500, #12000, #16144, #8338 ) ) ;
#12802 = CARTESIAN_POINT ( 'NONE',  ( -0.3334645669291338987, 9.254566434606299706E-06, -2.341456692880161228 ) ) ;
#12803 = CARTESIAN_POINT ( 'NONE',  ( -0.7217751814613770911, -0.1639319465203265547, 0.2161412452679343787 ) ) ;
#12804 = ORIENTED_EDGE ( 'NONE', *, *, #14808, .F. ) ;
#12805 = CARTESIAN_POINT ( 'NONE',  ( 0.4921259842519685179, 5.975917486140575174E-17, -1.550196850393700920 ) ) ;
#12806 = CIRCLE ( 'NONE', #7838, 1.288838582677165556 ) ;
#12807 = CARTESIAN_POINT ( 'NONE',  ( -0.2602238532265429005, 0.000000000000000000, -0.2362204724409449064 ) ) ;
#12808 = CARTESIAN_POINT ( 'NONE',  ( -0.3855916753051542023, -0.3382184156732014890, 1.766732283464566899 ) ) ;
#12809 = CARTESIAN_POINT ( 'NONE',  ( -0.5118110236220472231, -0.03349795313264326835, 1.747047244094488194 ) ) ;
#12810 = VERTEX_POINT ( 'NONE', #4102 ) ;
#12811 = ORIENTED_EDGE ( 'NONE', *, *, #22158, .T. ) ;
#12813 = CARTESIAN_POINT ( 'NONE',  ( 0.2842490391651533721, -0.2180698645301867300, -3.115157480314960647 ) ) ;
#12812 = CARTESIAN_POINT ( 'NONE',  ( 0.2952755905264887182, 0.000000000000000000, 2.090530474040783682E-11 ) ) ;
#12814 = ORIENTED_EDGE ( 'NONE', *, *, #7789, .T. ) ;
#12815 = CARTESIAN_POINT ( 'NONE',  ( 0.4585215200179055817, -2.840735999735804609E-17, -1.928289503579156516 ) ) ;
#12816 = VERTEX_POINT ( 'NONE', #23333 ) ;
#12817 = CARTESIAN_POINT ( 'NONE',  ( 0.3561571326799479742, 1.175382753584212514, -0.5166459152402519406 ) ) ;
#12818 = AXIS2_PLACEMENT_3D ( 'NONE', #12875, #6806, #23908 ) ;
#12819 = CARTESIAN_POINT ( 'NONE',  ( -0.2904160862623646477, -0.1677079028045411757, 1.973425196850393970 ) ) ;
#12820 = ORIENTED_EDGE ( 'NONE', *, *, #2360, .F. ) ;
#12821 = ORIENTED_EDGE ( 'NONE', *, *, #14034, .T. ) ;
#12822 = EDGE_CURVE ( 'NONE', #1472, #6364, #27173, .T. ) ;
#12823 = CARTESIAN_POINT ( 'NONE',  ( 0.1275996891957731083, 0.4763861460130595082, -1.550196850393700920 ) ) ;
#12824 = FACE_OUTER_BOUND ( 'NONE', #24726, .T. ) ;
#12825 = VERTEX_POINT ( 'NONE', #18922 ) ;
#12826 = ORIENTED_EDGE ( 'NONE', *, *, #9823, .T. ) ;
#12827 = EDGE_LOOP ( 'NONE', ( #13361, #7758, #19041, #6370 ) ) ;
#12828 = CARTESIAN_POINT ( 'NONE',  ( -0.1786951194748074845, 0.7326758143707651216, -0.6802888381025230524 ) ) ;
#12829 = EDGE_CURVE ( 'NONE', #11663, #8989, #13178, .T. ) ;
#12830 = AXIS2_PLACEMENT_3D ( 'NONE', #15828, #5080, #4950 ) ;
#12831 = CONTEXT_DEPENDENT_SHAPE_REPRESENTATION ( #22981, #814 ) ;
#12832 = CARTESIAN_POINT ( 'NONE',  ( 0.3976891862754212137, 0.8566358266442657410, -0.5893543329197449276 ) ) ;
#12833 = AXIS2_PLACEMENT_3D ( 'NONE', #22936, #14469, #23078 ) ;
#12834 = DIRECTION ( 'NONE',  ( -0.9009688679024190350, -0.4338837391175581759, 0.000000000000000000 ) ) ;
#12835 = B_SPLINE_CURVE_WITH_KNOTS ( 'NONE', 3,
 ( #7202, #2944, #11163, #15685, #13288, #572, #5213, #11574 ),
 .UNSPECIFIED., .F., .F.,
 ( 4, 2, 2, 4 ),
 ( 5.336250286839431171E-07, 0.0004434172983718084209, 0.0008863009717149328238, 0.001772068318401181846 ),
 .UNSPECIFIED. ) ;
#12836 = CARTESIAN_POINT ( 'NONE',  ( 0.3105951325284482811, -0.1787383246579994367, 0.1805249803478745085 ) ) ;
#12837 = ITEM_DEFINED_TRANSFORMATION ( 'NONE', 'NONE', #10711,  #11588 ) ;
#12838 = CIRCLE ( 'NONE', #6978, 0.5531496062992126150 ) ;
#12839 = CARTESIAN_POINT ( 'NONE',  ( -0.6299212598425196763, -0.4724409448818898127, -0.6411263657805729155 ) ) ;
#12840 = CARTESIAN_POINT ( 'NONE',  ( 0.1288129352161813124, 0.4793172621399190980, -1.569881889763779625 ) ) ;
#12841 = DIRECTION ( 'NONE',  ( -0.9848077530122077983, 0.1736481776669313304, 0.000000000000000000 ) ) ;
#12842 = VECTOR ( 'NONE', #18918, 39.37007874015748143 ) ;
#12843 = CARTESIAN_POINT ( 'NONE',  ( 0.04838950581351087604, 0.1968503937007873850, -3.209671902477004402 ) ) ;
#12844 = ORIENTED_EDGE ( 'NONE', *, *, #2597, .T. ) ;
#12845 = CIRCLE ( 'NONE', #2020, 0.1771653543307086520 ) ;
#12846 = VERTEX_POINT ( 'NONE', #10301 ) ;
#12847 = CARTESIAN_POINT ( 'NONE',  ( 0.3218523081042760081, -0.6665164569853854193, 0.2161412452716660326 ) ) ;
#12848 = SHAPE_REPRESENTATION_RELATIONSHIP ( 'NONE' , 'NONE' ,  #13162, #8334 ) ;
#12849 = VERTEX_POINT ( 'NONE', #3815 ) ;
#12850 = EDGE_CURVE ( 'NONE', #12810, #88, #21045, .T. ) ;
#12851 = FACE_BOUND ( 'NONE', #9124, .T. ) ;
#12852 = CARTESIAN_POINT ( 'NONE',  ( 2.048885995248197414E-16, 0.000000000000000000, 0.5532930914870255457 ) ) ;
#12853 = ORIENTED_EDGE ( 'NONE', *, *, #4650, .F. ) ;
#12854 = ADVANCED_FACE ( 'NONE', ( #3959, #16291 ), #21195, .T. ) ;
#12855 = AXIS2_PLACEMENT_3D ( 'NONE', #22569, #7884, #9555 ) ;
#12856 = CARTESIAN_POINT ( 'NONE',  ( -0.6562077975700374433, -2.731848031496062854E-17, 0.1574803149606299191 ) ) ;
#12857 = EDGE_LOOP ( 'NONE', ( #2963, #3681 ) ) ;
#12858 = CARTESIAN_POINT ( 'NONE',  ( -0.4337933494688747671, -0.2502226818840338485, 0.09684793308443542803 ) ) ;
#12859 = CARTESIAN_POINT ( 'NONE',  ( 0.2230788859036006988, 0.2650812153444456754, 0.1478915661146933680 ) ) ;
#12860 = ( REPRESENTATION_RELATIONSHIP ('NONE','NONE', #12434, #9188 ) REPRESENTATION_RELATIONSHIP_WITH_TRANSFORMATION ( #15654 )SHAPE_REPRESENTATION_RELATIONSHIP( ) ) ;
#12861 = CARTESIAN_POINT ( 'NONE',  ( 0.4162944719209874522, 0.3316996361851579089, 0.1322810039474933141 ) ) ;
#12862 = CARTESIAN_POINT ( 'NONE',  ( 0.000000000000000000, 0.000000000000000000, 0.1377952755905511861 ) ) ;
#12863 = CARTESIAN_POINT ( 'NONE',  ( -0.4247824284860164945, 0.000000000000000000, -0.04133858267716535029 ) ) ;
#12864 = APPLICATION_CONTEXT ( 'automotive_design' ) ;
#12865 = AXIS2_PLACEMENT_3D ( 'NONE', #19631, #17496, #6773 ) ;
#12866 = ORIENTED_EDGE ( 'NONE', *, *, #18277, .F. ) ;
#12867 = CARTESIAN_POINT ( 'NONE',  ( 0.000000000000000000, 0.000000000000000000, -4.209669677817527322 ) ) ;
#12868 = CARTESIAN_POINT ( 'NONE',  ( 8.810208661417323492E-17, -4.420669291338583154E-18, 0.000000000000000000 ) ) ;
#12869 = CARTESIAN_POINT ( 'NONE',  ( -0.1771653543307086520, -0.5570866141732283561, 6.822343388950805452E-17 ) ) ;
#12870 = DIRECTION ( 'NONE',  ( 1.000000000000000000, 0.000000000000000000, 0.000000000000000000 ) ) ;
#12871 = CARTESIAN_POINT ( 'NONE',  ( -8.919671568592927398E-17, -0.7283464566929134243, 0.1771653543307086520 ) ) ;
#12872 = LINE ( 'NONE', #15157, #2369 ) ;
#12873 = CARTESIAN_POINT ( 'NONE',  ( 0.3334645669291338987, -0.7876517371453680694, -0.8174568431611989316 ) ) ;
#12874 = CARTESIAN_POINT ( 'NONE',  ( -0.3642352168757849173, -0.4152525734086955356, 0.9399606299212598381 ) ) ;
#12875 = CARTESIAN_POINT ( 'NONE',  ( 0.000000000000000000, 0.8661417322803149910, 0.000000000000000000 ) ) ;
#12876 = CARTESIAN_POINT ( 'NONE',  ( -0.3574975638436101444, 0.000000000000000000, -3.115157480314960647 ) ) ;
#12877 = VECTOR ( 'NONE', #12981, 39.37007874015748143 ) ;
#12878 = ORIENTED_EDGE ( 'NONE', *, *, #23187, .F. ) ;
#12879 = B_SPLINE_CURVE_WITH_KNOTS ( 'NONE', 3,
 ( #8458, #10569, #10855, #8598, #10286, #18902 ),
 .UNSPECIFIED., .F., .F.,
 ( 4, 2, 4 ),
 ( 0.5000000000000000000, 0.7500000000000000000, 1.000000000000000000 ),
 .UNSPECIFIED. ) ;
#12880 = ORIENTED_EDGE ( 'NONE', *, *, #20059, .F. ) ;
#12881 = CARTESIAN_POINT ( 'NONE',  ( -0.3855916753034290823, 0.3382184156749268311, -1.550196850393700920 ) ) ;
#12882 = DIRECTION ( 'NONE',  ( 0.000000000000000000, 0.000000000000000000, 1.000000000000000000 ) ) ;
#12883 = CIRCLE ( 'NONE', #21929, 0.6212598425196850238 ) ;
#12884 = CARTESIAN_POINT ( 'NONE',  ( 0.1580799066051618851, -0.4326553680327471785, 0.1771653543307085410 ) ) ;
#12885 = CARTESIAN_POINT ( 'NONE',  ( 0.000000000000000000, 0.07874015748031495954, 0.000000000000000000 ) ) ;
#12886 = FACE_OUTER_BOUND ( 'NONE', #15656, .T. ) ;
#12887 = ORIENTED_EDGE ( 'NONE', *, *, #12765, .F. ) ;
#12888 = EDGE_CURVE ( 'NONE', #5007, #19599, #5551, .T. ) ;
#12889 = DIRECTION ( 'NONE',  ( 1.000000000000000000, 0.000000000000000000, 0.000000000000000000 ) ) ;
#12890 = ORIENTED_EDGE ( 'NONE', *, *, #5935, .T. ) ;
#12891 = ORIENTED_EDGE ( 'NONE', *, *, #19240, .F. ) ;
#12892 = AXIS2_PLACEMENT_3D ( 'NONE', #8547, #17433, #21818 ) ;
#12893 = CARTESIAN_POINT ( 'NONE',  ( -5.747161356628524594E-17, -0.4692913385826771866, 0.1992125984251968684 ) ) ;
#12894 = CARTESIAN_POINT ( 'NONE',  ( -0.4792483803599256187, 0.08390985360213192024, 0.1075369453628696598 ) ) ;
#12895 = CARTESIAN_POINT ( 'NONE',  ( 0.3665264996331779601, -0.2116141732283464416, 0.1377952755905511861 ) ) ;
#12896 = ORIENTED_EDGE ( 'NONE', *, *, #27181, .T. ) ;
#12897 = CIRCLE ( 'NONE', #16961, 0.1308464566929133932 ) ;
#12898 = CARTESIAN_POINT ( 'NONE',  ( 0.000000000000000000, 0.000000000000000000, -0.04133858267716535029 ) ) ;
#12899 = CARTESIAN_POINT ( 'NONE',  ( -0.02559055118110236185, -0.8267716535433071723, 1.012503259137575512E-16 ) ) ;
#12900 = ORIENTED_EDGE ( 'NONE', *, *, #12647, .T. ) ;
#12901 = CARTESIAN_POINT ( 'NONE',  ( 0.000000000000000000, -1.533249767903113305E-16, 0.000000000000000000 ) ) ;
#12902 = ORIENTED_EDGE ( 'NONE', *, *, #23103, .T. ) ;
#12903 = CARTESIAN_POINT ( 'NONE',  ( -0.4527559054764770385, 0.000000000000000000, -1.934055118110236338 ) ) ;
#12904 = B_SPLINE_CURVE_WITH_KNOTS ( 'NONE', 3,
 ( #10721, #21467, #21600, #6488 ),
 .UNSPECIFIED., .F., .F.,
 ( 4, 4 ),
 ( 0.001747226565907129044, 0.002631077521236949331 ),
 .UNSPECIFIED. ) ;
#12905 = CARTESIAN_POINT ( 'NONE',  ( 0.2268967137093004516, -0.4599980997183342746, -1.550196850393700920 ) ) ;
#12906 = CONICAL_SURFACE ( 'NONE', #7040, 0.06200787401574805319, 1.029744258088332254 ) ;
#12907 = ADVANCED_FACE ( 'NONE', ( #25573 ), #16819, .T. ) ;
#12908 = CARTESIAN_POINT ( 'NONE',  ( 0.1706130639248417957, -0.4670119966435259951, 0.1615162260935599503 ) ) ;
#12909 = AXIS2_PLACEMENT_3D ( 'NONE', #27597, #6404, #21785 ) ;
#12910 = CARTESIAN_POINT ( 'NONE',  ( -0.5252801253069795395, -0.2960335176359168985, -0.2916644167427649981 ) ) ;
#12911 = PRESENTATION_STYLE_ASSIGNMENT (( #21957 ) ) ;
#12912 = PLANE ( 'NONE',  #27871 ) ;
#12913 = DIRECTION ( 'NONE',  ( 0.000000000000000000, 1.000000000000000000, 0.000000000000000000 ) ) ;
#12914 = DIRECTION ( 'NONE',  ( 0.000000000000000000, 0.000000000000000000, 1.000000000000000000 ) ) ;
#12915 = ADVANCED_FACE ( 'NONE', ( #11573 ), #27223, .T. ) ;
#12916 = CARTESIAN_POINT ( 'NONE',  ( 0.6299212598425196763, 0.07910393700787400617, 1.087052427555504903E-17 ) ) ;
#12917 = CARTESIAN_POINT ( 'NONE',  ( -0.2937497900409605234, 0.3350145293473837382, -1.934055118110236338 ) ) ;
#12918 = CARTESIAN_POINT ( 'NONE',  ( -0.7432982829791772161, 0.2424461424275303201, -0.1088776918758622148 ) ) ;
#12919 = VERTEX_POINT ( 'NONE', #16765 ) ;
#12920 = DIRECTION ( 'NONE',  ( 0.000000000000000000, 1.000000000000000000, 0.000000000000000000 ) ) ;
#12921 = CARTESIAN_POINT ( 'NONE',  ( -0.5376957092749645728, -0.3112026930392425284, 0.09685039370078740717 ) ) ;
#12922 = CARTESIAN_POINT ( 'NONE',  ( -0.5417097841048799101, -0.1839420097223198047, 0.9399606299212598381 ) ) ;
#12923 = AXIS2_PLACEMENT_3D ( 'NONE', #19843, #17708, #26062 ) ;
#12924 = PLANE ( 'NONE',  #4556 ) ;
#12925 = CIRCLE ( 'NONE', #5729, 0.1181102362204720091 ) ;
#12926 = CARTESIAN_POINT ( 'NONE',  ( -0.1153557615297513411, -0.4303681241737880026, -1.934055118110236338 ) ) ;
#12927 = CARTESIAN_POINT ( 'NONE',  ( -0.02438677169350799909, 0.3726024258163779246, -3.115157480314960647 ) ) ;
#12928 = DIRECTION ( 'NONE',  ( 0.000000000000000000, 0.000000000000000000, 1.000000000000000000 ) ) ;
#12929 = CARTESIAN_POINT ( 'NONE',  ( -0.4724409448465559103, 0.000000000000000000, 1.953740157480315043 ) ) ;
#12930 = CARTESIAN_POINT ( 'NONE',  ( -0.1771653543307086520, -5.663984251968503442E-18, 0.000000000000000000 ) ) ;
#12931 = DIRECTION ( 'NONE',  ( 0.000000000000000000, 0.000000000000000000, -1.000000000000000000 ) ) ;
#12932 = CARTESIAN_POINT ( 'NONE',  ( -0.1771653543307086520, 0.7539370078740157410, 0.000000000000000000 ) ) ;
#12933 = ADVANCED_FACE ( 'NONE', ( #7872 ), #13691, .F. ) ;
#12934 = VERTEX_POINT ( 'NONE', #14240 ) ;
#12935 = EDGE_LOOP ( 'NONE', ( #8170, #21850, #5788, #3933 ) ) ;
#12936 = ORIENTED_EDGE ( 'NONE', *, *, #5472, .T. ) ;
#12937 = AXIS2_PLACEMENT_3D ( 'NONE', #17382, #192, #15283 ) ;
#12938 = EDGE_CURVE ( 'NONE', #12118, #18288, #4938, .T. ) ;
#12939 = ORIENTED_EDGE ( 'NONE', *, *, #6949, .F. ) ;
#12940 = DIRECTION ( 'NONE',  ( -0.000000000000000000, -1.000000000000000000, -0.000000000000000000 ) ) ;
#12941 = FACE_OUTER_BOUND ( 'NONE', #7930, .T. ) ;
#12942 = CARTESIAN_POINT ( 'NONE',  ( 0.03349795313264414959, -0.5118110236220471121, 1.766732283464566899 ) ) ;
#12943 = ADVANCED_FACE ( 'NONE', ( #15819, #1507 ), #22993, .F. ) ;
#12944 = CARTESIAN_POINT ( 'NONE',  ( -0.3382184156732160329, -0.3855916753051698009, 1.747047244094488194 ) ) ;
#12945 = CARTESIAN_POINT ( 'NONE',  ( 8.741913385826771462E-17, 0.1328740157480315098, 0.000000000000000000 ) ) ;
#12946 = ORIENTED_EDGE ( 'NONE', *, *, #4001, .F. ) ;
#12947 = VERTEX_POINT ( 'NONE', #24426 ) ;
#12949 = CARTESIAN_POINT ( 'NONE',  ( -0.3574975638436101444, 0.000000000000000000, -3.115157480314960647 ) ) ;
#12948 = DIRECTION ( 'NONE',  ( 0.000000000000000000, 1.000000000000000000, 0.000000000000000000 ) ) ;
#12950 = ORIENTED_EDGE ( 'NONE', *, *, #9446, .T. ) ;
#12951 = ADVANCED_FACE ( 'NONE', ( #12243 ), #22174, .F. ) ;
#12952 = ORIENTED_EDGE ( 'NONE', *, *, #5362, .F. ) ;
#12953 = CARTESIAN_POINT ( 'NONE',  ( 0.000000000000000000, 0.000000000000000000, 0.2637795275590551491 ) ) ;
#12954 = DIRECTION ( 'NONE',  ( 1.000000000000000000, 0.000000000000000000, 0.000000000000000000 ) ) ;
#12955 = CARTESIAN_POINT ( 'NONE',  ( 0.2660793235464269380, 0.2041304421298361926, 1.973425196850393970 ) ) ;
#12956 = VERTEX_POINT ( 'NONE', #5070 ) ;
#12957 = ORIENTED_EDGE ( 'NONE', *, *, #23, .F. ) ;
#12958 = LINE ( 'NONE', #6068, #15639 ) ;
#12959 = DIRECTION ( 'NONE',  ( 0.000000000000000000, 0.000000000000000000, -1.000000000000000000 ) ) ;
#12960 = ORIENTED_EDGE ( 'NONE', *, *, #14743, .F. ) ;
#12961 = ORIENTED_EDGE ( 'NONE', *, *, #18615, .F. ) ;
#12962 = ORIENTED_EDGE ( 'NONE', *, *, #3694, .F. ) ;
#12963 = AXIS2_PLACEMENT_3D ( 'NONE', #1450, #27308, #22646 ) ;
#12964 = DIRECTION ( 'NONE',  ( 0.000000000000000000, 0.000000000000000000, -1.000000000000000000 ) ) ;
#12965 = DIRECTION ( 'NONE',  ( 0.000000000000000000, 0.000000000000000000, 1.000000000000000000 ) ) ;
#12966 = CIRCLE ( 'NONE', #788, 0.3771653543307086909 ) ;
#12967 = VERTEX_POINT ( 'NONE', #2800 ) ;
#12968 = CARTESIAN_POINT ( 'NONE',  ( 0.4895436826824360321, 0.08692528595286251603, 0.1140743250917607421 ) ) ;
#12969 = VERTEX_POINT ( 'NONE', #9300 ) ;
#12970 = B_SPLINE_SURFACE_WITH_KNOTS ( 'NONE', 2, 3, ( 
 ( #14350, #11794, #22963, #5583 ),
 ( #25069, #11940, #5147, #1073 ),
 ( #13774, #27058, #26911, #5733 ) ),
 .UNSPECIFIED., .F., .F., .F.,
 ( 3, 3 ),
 ( 4, 4 ),
 ( 0.000000000000000000, 1.000000000000000000 ),
 ( -0.006999999999999992339, -1.387778780781445676E-17 ),
 .UNSPECIFIED. ) ;
#12971 = ( GEOMETRIC_REPRESENTATION_CONTEXT ( 3 ) GLOBAL_UNCERTAINTY_ASSIGNED_CONTEXT ( ( #11578 ) ) GLOBAL_UNIT_ASSIGNED_CONTEXT ( ( #21537, #19558, #21813 ) ) REPRESENTATION_CONTEXT ( 'NONE', 'WORKASPACE' ) ) ;
#12972 = DIRECTION ( 'NONE',  ( -1.000000000000000000, 0.000000000000000000, 0.000000000000000000 ) ) ;
#12973 = LINE ( 'NONE', #10858, #15072 ) ;
#12974 = EDGE_CURVE ( 'NONE', #22865, #25110, #12725, .T. ) ;
#12975 = CARTESIAN_POINT ( 'NONE',  ( -0.3613813581019308385, -1.111881281712430614, -0.4008318706050917335 ) ) ;
#12976 = CARTESIAN_POINT ( 'NONE',  ( 0.000000000000000000, 0.000000000000000000, -0.4724409448818898127 ) ) ;
#12977 = FACE_OUTER_BOUND ( 'NONE', #20455, .T. ) ;
#12978 = DIRECTION ( 'NONE',  ( 1.000000000000000000, 0.000000000000000000, 0.000000000000000000 ) ) ;
#12979 = CYLINDRICAL_SURFACE ( 'NONE', #23228, 0.8163976377952756325 ) ;
#12980 = ADVANCED_FACE ( 'NONE', ( #9979 ), #22312, .F. ) ;
#12981 = DIRECTION ( 'NONE',  ( -1.000000000000000000, 0.000000000000000000, 0.000000000000000000 ) ) ;
#12982 = ORIENTED_EDGE ( 'NONE', *, *, #24353, .T. ) ;
#12983 = PRODUCT_DEFINITION_FORMATION_WITH_SPECIFIED_SOURCE ( 'ANY', '', #23113, .NOT_KNOWN. ) ;
#12984 = DIRECTION ( 'NONE',  ( -1.000000000000000000, 0.000000000000000000, 0.000000000000000000 ) ) ;
#12985 = ( LENGTH_UNIT ( ) NAMED_UNIT ( * ) SI_UNIT ( $, .METRE. ) ) ;
#12986 = VERTEX_POINT ( 'NONE', #18868 ) ;
#12987 = CIRCLE ( 'NONE', #10005, 1.092519685039370136 ) ;
#12988 = CARTESIAN_POINT ( 'NONE',  ( -0.1669561253486535057, -0.4569961989591353468, 0.1075369453278852555 ) ) ;
#12989 = CARTESIAN_POINT ( 'NONE',  ( -0.5700941239023215035, 1.111319899718911985, -0.06074667524653134393 ) ) ;
#12990 = CARTESIAN_POINT ( 'NONE',  ( -0.4527559055118110520, 0.000000000000000000, 0.000000000000000000 ) ) ;
#12991 = ORIENTED_EDGE ( 'NONE', *, *, #15404, .T. ) ;
#12992 = CARTESIAN_POINT ( 'NONE',  ( -0.1775991818008590406, -0.5230301363771331369, 0.9202755905511811330 ) ) ;
#12993 = DIRECTION ( 'NONE',  ( 0.000000000000000000, -1.000000000000000000, 0.000000000000000000 ) ) ;
#12994 = ORIENTED_EDGE ( 'NONE', *, *, #25094, .F. ) ;
#12995 = ADVANCED_FACE ( 'NONE', ( #18732 ), #6423, .T. ) ;
#12996 = DIRECTION ( 'NONE',  ( -1.000000000000000000, 0.000000000000000000, 0.000000000000000000 ) ) ;
#12997 = FACE_OUTER_BOUND ( 'NONE', #4601, .T. ) ;
#12998 = B_SPLINE_CURVE_WITH_KNOTS ( 'NONE', 3,
 ( #4654, #12859, #10597, #4116, #19363, #62 ),
 .UNSPECIFIED., .F., .F.,
 ( 4, 2, 4 ),
 ( 0.5000000000000000000, 0.7500000000000000000, 1.000000000000000000 ),
 .UNSPECIFIED. ) ;
#12999 = DIRECTION ( 'NONE',  ( 0.000000000000000000, 1.000000000000000000, 0.000000000000000000 ) ) ;
#13000 = DIRECTION ( 'NONE',  ( -1.000000000000000000, 0.000000000000000000, 0.000000000000000000 ) ) ;
#13001 = DIRECTION ( 'NONE',  ( 0.000000000000000000, 0.000000000000000000, 1.000000000000000000 ) ) ;
#13002 = AXIS2_PLACEMENT_3D ( 'NONE', #847, #24694, #20050 ) ;
#13003 = AXIS2_PLACEMENT_3D ( 'NONE', #13876, #22073, #9772 ) ;
#13004 = CARTESIAN_POINT ( 'NONE',  ( 0.1570092758121679200, -0.4330450457732857861, 0.1771653543307087630 ) ) ;
#13005 = AXIS2_PLACEMENT_3D ( 'NONE', #14939, #12233, #3898 ) ;
#13006 = LINE ( 'NONE', #19370, #17391 ) ;
#13007 = CARTESIAN_POINT ( 'NONE',  ( 0.5572789388074469441, -0.3225230913461603066, 0.1183902030391640881 ) ) ;
#13008 = CYLINDRICAL_SURFACE ( 'NONE', #19783, 0.1181102362204720091 ) ;
#13009 = DIRECTION ( 'NONE',  ( -1.000000000000000000, 0.000000000000000000, 0.000000000000000000 ) ) ;
#13010 = CARTESIAN_POINT ( 'NONE',  ( 0.000000000000000000, 0.000000000000000000, -0.2204724409448818867 ) ) ;
#13011 = EDGE_CURVE ( 'NONE', #333, #25553, #2779, .T. ) ;
#13012 = CARTESIAN_POINT ( 'NONE',  ( 0.1480156394741987402, 0.5526079293737075071, 0.9399606299212598381 ) ) ;
#13013 = EDGE_CURVE ( 'NONE', #3201, #27168, #4161, .T. ) ;
#13014 = AXIS2_PLACEMENT_3D ( 'NONE', #16125, #15576, #24181 ) ;
#13015 = CYLINDRICAL_SURFACE ( 'NONE', #23667, 1.288838582677165556 ) ;
#13016 = VERTEX_POINT ( 'NONE', #3762 ) ;
#13017 = LINE ( 'NONE', #23636, #6966 ) ;
#13018 = EDGE_CURVE ( 'NONE', #16237, #15239, #1646, .T. ) ;
#13019 = ORIENTED_EDGE ( 'NONE', *, *, #6413, .F. ) ;
#13020 = ORIENTED_EDGE ( 'NONE', *, *, #22197, .T. ) ;
#13021 = AXIS2_PLACEMENT_3D ( 'NONE', #19330, #10997, #27820 ) ;
#13022 = ORIENTED_EDGE ( 'NONE', *, *, #23764, .F. ) ;
#13023 = VECTOR ( 'NONE', #15601, 39.37007874015748143 ) ;
#13024 = CARTESIAN_POINT ( 'NONE',  ( 0.4600326175570071952, 0.2268096725200290653, -1.550196850393700920 ) ) ;
#13025 = CARTESIAN_POINT ( 'NONE',  ( -0.5130740159360542840, -0.2530785775248223235, 0.9399606299212598381 ) ) ;
#13026 = CARTESIAN_POINT ( 'NONE',  ( 0.4622619257814346572, 0.08092139668567618904, 0.07637795275590551769 ) ) ;
#13027 = AXIS2_PLACEMENT_3D ( 'NONE', #24670, #24820, #22426 ) ;
#13028 = ORIENTED_EDGE ( 'NONE', *, *, #17207, .T. ) ;
#13029 = FACE_OUTER_BOUND ( 'NONE', #3523, .T. ) ;
#13030 = DIRECTION ( 'NONE',  ( 0.000000000000000000, -1.000000000000000000, 0.000000000000000000 ) ) ;
#13031 = EDGE_LOOP ( 'NONE', ( #9379, #18411, #25686, #6258 ) ) ;
#13032 = ADVANCED_FACE ( 'NONE', ( #12384 ), #2943, .T. ) ;
#13033 = DIRECTION ( 'NONE',  ( 0.000000000000000000, 0.000000000000000000, -1.000000000000000000 ) ) ;
#13034 = AXIS2_PLACEMENT_3D ( 'NONE', #17239, #23748, #27210 ) ;
#13035 = FACE_OUTER_BOUND ( 'NONE', #22546, .T. ) ;
#13036 = DIRECTION ( 'NONE',  ( 1.000000000000000000, 5.737213000000000442E-16, 0.000000000000000000 ) ) ;
#13037 = B_SPLINE_CURVE_WITH_KNOTS ( 'NONE', 3,
 ( #16742, #4308, #15219, #25504 ),
 .UNSPECIFIED., .F., .F.,
 ( 4, 4 ),
 ( 1.006307675027575899, 1.007953978091874037 ),
 .UNSPECIFIED. ) ;
#13038 = ORIENTED_EDGE ( 'NONE', *, *, #20852, .F. ) ;
#13039 = CARTESIAN_POINT ( 'NONE',  ( 0.000000000000000000, 0.000000000000000000, 0.1377952755905511861 ) ) ;
#13040 = LINE ( 'NONE', #19811, #17571 ) ;
#13041 = ORIENTED_EDGE ( 'NONE', *, *, #27618, .T. ) ;
#13042 = DIRECTION ( 'NONE',  ( 0.000000000000000000, 1.000000000000000000, 0.000000000000000000 ) ) ;
#13043 = DIRECTION ( 'NONE',  ( 0.000000000000000000, -1.000000000000000000, 0.000000000000000000 ) ) ;
#13044 = CARTESIAN_POINT ( 'NONE',  ( 0.03220957031753989008, 0.4921259842519685179, -1.550196850393700920 ) ) ;
#13045 = DIMENSIONAL_EXPONENTS ( 1.000000000000000000, 0.000000000000000000, 0.000000000000000000, 0.000000000000000000, 0.000000000000000000, 0.000000000000000000, 0.000000000000000000 ) ;
#13046 = CIRCLE ( 'NONE', #18423, 0.5322834645669292097 ) ;
#13047 = CARTESIAN_POINT ( 'NONE',  ( 0.1458850421962665789, 0.4296318976990154970, -1.934055118110236338 ) ) ;
#13048 = VECTOR ( 'NONE', #21673, 39.37007874015748143 ) ;
#13049 = CIRCLE ( 'NONE', #22074, 0.1308464566929133932 ) ;
#13050 = ADVANCED_FACE ( 'NONE', ( #9439 ), #20853, .T. ) ;
#13051 = DIRECTION ( 'NONE',  ( 0.000000000000000000, 1.000000000000000000, 0.000000000000000000 ) ) ;
#13052 = CARTESIAN_POINT ( 'NONE',  ( 0.1715719712208858272, -0.4696414150079809002, 0.1496602734630888831 ) ) ;
#13053 = EDGE_CURVE ( 'NONE', #20876, #21486, #19943, .T. ) ;
#13054 = PRESENTATION_LAYER_ASSIGNMENT (  '', '', ( #18434 ) ) ;
#13055 = CARTESIAN_POINT ( 'NONE',  ( -0.4055118110236220486, -0.4724409448818898127, -0.6874452634183682020 ) ) ;
#13056 = CARTESIAN_POINT ( 'NONE',  ( 0.3223547283257516272, 0.3832433309296771617, 0.09685039370078740717 ) ) ;
#13057 = CARTESIAN_POINT ( 'NONE',  ( -0.6594488188976378451, 0.000000000000000000, -3.993519685039370632E-17 ) ) ;
#13058 = DIRECTION ( 'NONE',  ( 0.000000000000000000, 1.000000000000000000, 0.000000000000000000 ) ) ;
#13059 = CARTESIAN_POINT ( 'NONE',  ( -0.3543307086614173596, 4.268512490100411279E-17, 1.953740157480315043 ) ) ;
#13060 = DIRECTION ( 'NONE',  ( 0.000000000000000000, 0.000000000000000000, -1.000000000000000000 ) ) ;
#13061 = CARTESIAN_POINT ( 'NONE',  ( 0.3995066426835866547, 0.4757712504659488140, 0.2574827755769819038 ) ) ;
#13062 = VERTEX_POINT ( 'NONE', #10538 ) ;
#13063 = CONICAL_SURFACE ( 'NONE', #4039, 0.4724409448818898127, 0.7853981625000003852 ) ;
#13064 = CARTESIAN_POINT ( 'NONE',  ( 0.3429980251342297226, -0.09187177619658888628, 1.953740157480315043 ) ) ;
#13065 = ORIENTED_EDGE ( 'NONE', *, *, #14772, .T. ) ;
#13066 = CARTESIAN_POINT ( 'NONE',  ( -0.1458850421962410715, 0.4296318976989903504, -1.934055118110236338 ) ) ;
#13067 = FACE_OUTER_BOUND ( 'NONE', #14921, .T. ) ;
#13068 = VECTOR ( 'NONE', #24575, 39.37007874015748143 ) ;
#13069 = CARTESIAN_POINT ( 'NONE',  ( -8.427884271297532088E-17, -0.6881889763779527325, 0.4724409448818898127 ) ) ;
#13070 = CARTESIAN_POINT ( 'NONE',  ( -0.07874015748031495954, -0.04546065111729338803, -0.3779527559055118058 ) ) ;
#13071 = ( REPRESENTATION_RELATIONSHIP ('NONE','NONE', #12434, #13162 ) REPRESENTATION_RELATIONSHIP_WITH_TRANSFORMATION ( #8542 )SHAPE_REPRESENTATION_RELATIONSHIP( ) ) ;
#13072 = DIRECTION ( 'NONE',  ( 0.000000000000000000, 1.000000000000000000, 0.000000000000000000 ) ) ;
#13073 = EDGE_CURVE ( 'NONE', #15131, #4007, #12282, .T. ) ;
#13074 = CARTESIAN_POINT ( 'NONE',  ( -0.2146455952181789972, -0.4472013107399995802, 0.2989974301012601199 ) ) ;
#13075 = CARTESIAN_POINT ( 'NONE',  ( 0.3233561589689049054, 0.1867299569291689110, -3.115157480314960647 ) ) ;
#13076 = DIRECTION ( 'NONE',  ( 0.000000000000000000, 1.000000000000000000, 0.000000000000000000 ) ) ;
#13077 = CARTESIAN_POINT ( 'NONE',  ( 0.3065394984556240598, 0.3644188803044271507, 0.1212655228622371850 ) ) ;
#13078 = VERTEX_POINT ( 'NONE', #15216 ) ;
#13079 = LINE ( 'NONE', #8428, #4611 ) ;
#13080 = AXIS2_PLACEMENT_3D ( 'NONE', #16305, #27185, #20395 ) ;
#13081 = VERTEX_POINT ( 'NONE', #12932 ) ;
#13082 = CARTESIAN_POINT ( 'NONE',  ( 0.4921259842519685179, 2.987958743070287587E-17, -1.569881889763779625 ) ) ;
#13083 = CIRCLE ( 'NONE', #10374, 0.4606299212598425341 ) ;
#13084 = ORIENTED_EDGE ( 'NONE', *, *, #25064, .T. ) ;
#13085 = ORIENTED_EDGE ( 'NONE', *, *, #20373, .F. ) ;
#13086 = DIRECTION ( 'NONE',  ( 0.000000000000000000, 1.000000000000000000, 0.000000000000000000 ) ) ;
#13087 = CARTESIAN_POINT ( 'NONE',  ( 0.06699590632655395839, 0.5118110236220472231, 1.766732283464566899 ) ) ;
#13088 = CARTESIAN_POINT ( 'NONE',  ( -0.4954415918530857832, 0.1327036767659614813, 1.766732283464566899 ) ) ;
#13089 = ORIENTED_EDGE ( 'NONE', *, *, #17412, .F. ) ;
#13090 = AXIS2_PLACEMENT_3D ( 'NONE', #11459, #9465, #731 ) ;
#13091 = ORIENTED_EDGE ( 'NONE', *, *, #15192, .T. ) ;
#13092 = CARTESIAN_POINT ( 'NONE',  ( -0.2462256503455939050, 0.2807137536170327685, -3.115157480314960647 ) ) ;
#13093 = ORIENTED_EDGE ( 'NONE', *, *, #23388, .F. ) ;
#13094 = VERTEX_POINT ( 'NONE', #14946 ) ;
#13095 = FACE_OUTER_BOUND ( 'NONE', #6604, .T. ) ;
#13096 = DIRECTION ( 'NONE',  ( 1.000000000000000000, 0.000000000000000000, 0.000000000000000000 ) ) ;
#13097 = CARTESIAN_POINT ( 'NONE',  ( -0.04380447413658625222, -0.3324885138898230341, 1.953740157480315043 ) ) ;
#13098 = VERTEX_POINT ( 'NONE', #19586 ) ;
#13099 = ORIENTED_EDGE ( 'NONE', *, *, #5501, .F. ) ;
#13100 = EDGE_CURVE ( 'NONE', #2802, #14678, #575, .T. ) ;
#13101 = DIRECTION ( 'NONE',  ( 1.000000000000000000, 0.000000000000000000, 0.000000000000000000 ) ) ;
#13102 = ORIENTED_EDGE ( 'NONE', *, *, #14275, .T. ) ;
#13103 = ORIENTED_EDGE ( 'NONE', *, *, #5694, .F. ) ;
#13104 = ORIENTED_EDGE ( 'NONE', *, *, #19932, .T. ) ;
#13105 = CARTESIAN_POINT ( 'NONE',  ( -0.1706130639252569914, -0.4670119966446516502, 0.1140743250909571488 ) ) ;
#13106 = AXIS2_PLACEMENT_3D ( 'NONE', #8010, #25229, #1640 ) ;
#13107 = DIRECTION ( 'NONE',  ( 1.000000000000000000, 0.000000000000000000, 0.000000000000000000 ) ) ;
#13108 = CARTESIAN_POINT ( 'NONE',  ( -0.3048711895200191258, -0.6348424542969446360, 0.1443310008633306996 ) ) ;
#13109 = CARTESIAN_POINT ( 'NONE',  ( 0.5376957092749897749, -0.3112026930391976753, 0.2574803149606298969 ) ) ;
#13110 = EDGE_LOOP ( 'NONE', ( #3635, #2785, #22657, #1846, #13648, #13464 ) ) ;
#13111 = EDGE_CURVE ( 'NONE', #17618, #5784, #14815, .T. ) ;
#13112 = CONICAL_SURFACE ( 'NONE', #3165, 1.112204724409448842, 0.7853981625000011624 ) ;
#13113 = CARTESIAN_POINT ( 'NONE',  ( 0.000000000000000000, 0.000000000000000000, 0.1771653543307086520 ) ) ;
#13114 = EDGE_CURVE ( 'NONE', #19596, #24341, #23584, .T. ) ;
#13115 = DIRECTION ( 'NONE',  ( 1.000000000000000000, 0.000000000000000000, 0.000000000000000000 ) ) ;
#13116 = ORIENTED_EDGE ( 'NONE', *, *, #15401, .T. ) ;
#13117 = CARTESIAN_POINT ( 'NONE',  ( 2.632951206231566310, -0.4724409448818898127, -0.6874452634183682020 ) ) ;
#13118 = FACE_BOUND ( 'NONE', #4727, .T. ) ;
#13119 = CARTESIAN_POINT ( 'NONE',  ( -5.645730259564185549E-17, 0.4692913385826772976, 0.07637549214372836570 ) ) ;
#13120 = AXIS2_PLACEMENT_3D ( 'NONE', #24767, #9654, #25190 ) ;
#13121 = CARTESIAN_POINT ( 'NONE',  ( -0.07669076177803968442, 0.1968503937007873850, -3.252027725244194922 ) ) ;
#13122 = EDGE_LOOP ( 'NONE', ( #26926, #12425, #22002, #20164 ) ) ;
#13123 = DIRECTION ( 'NONE',  ( -1.000000000000000000, 0.000000000000000000, 0.000000000000000000 ) ) ;
#13124 = ORIENTED_EDGE ( 'NONE', *, *, #992, .T. ) ;
#13125 = CARTESIAN_POINT ( 'NONE',  ( -0.3289909311256229429, 0.1896185148830510925, -3.100567304031763172 ) ) ;
#13126 = AXIS2_PLACEMENT_3D ( 'NONE', #8148, #12517, #21280 ) ;
#13127 = DIRECTION ( 'NONE',  ( 0.000000000000000000, 0.000000000000000000, 1.000000000000000000 ) ) ;
#13128 = FACE_OUTER_BOUND ( 'NONE', #938, .T. ) ;
#13129 = CARTESIAN_POINT ( 'NONE',  ( 0.0007756954652704383529, 0.7174612052789276495, 0.3122824329332504201 ) ) ;
#13130 = VERTEX_POINT ( 'NONE', #21705 ) ;
#13131 = CARTESIAN_POINT ( 'NONE',  ( 0.2762247810519068980, 0.4783323773986306038, 0.9399606299212598381 ) ) ;
#13132 = CARTESIAN_POINT ( 'NONE',  ( 0.000000000000000000, 0.000000000000000000, 0.1992125984251968684 ) ) ;
#13133 = VERTEX_POINT ( 'NONE', #27788 ) ;
#13134 = EDGE_CURVE ( 'NONE', #5560, #20533, #19505, .T. ) ;
#13135 = CARTESIAN_POINT ( 'NONE',  ( 0.2307318466679419144, 0.2741888764719463967, 0.09506557084205286001 ) ) ;
#13136 = CARTESIAN_POINT ( 'NONE',  ( 0.000000000000000000, 0.000000000000000000, 0.1992125984251968684 ) ) ;
#13137 = DIRECTION ( 'NONE',  ( 0.000000000000000000, 0.000000000000000000, -1.000000000000000000 ) ) ;
#13138 = DIRECTION ( 'NONE',  ( 0.000000000000000000, 0.000000000000000000, -1.000000000000000000 ) ) ;
#13139 = EDGE_CURVE ( 'NONE', #15868, #20920, #13377, .T. ) ;
#13140 = DIRECTION ( 'NONE',  ( 1.000000000000000000, 0.000000000000000000, 0.000000000000000000 ) ) ;
#13141 = DIRECTION ( 'NONE',  ( 0.000000000000000000, -1.000000000000000000, 0.000000000000000000 ) ) ;
#13142 = CARTESIAN_POINT ( 'NONE',  ( 0.5692936381913840105, -0.3294684677436600095, 0.1461456498297685480 ) ) ;
#13143 = ADVANCED_FACE ( 'NONE', ( #4055 ), #2332, .F. ) ;
#13144 = DIRECTION ( 'NONE',  ( 1.000000000000000000, 0.000000000000000000, 0.000000000000000000 ) ) ;
#13145 = ORIENTED_EDGE ( 'NONE', *, *, #10157, .T. ) ;
#13146 = DIRECTION ( 'NONE',  ( -1.000000000000000000, 0.000000000000000000, 0.000000000000000000 ) ) ;
#13147 = AXIS2_PLACEMENT_3D ( 'NONE', #6602, #139, #19310 ) ;
#13148 = TOROIDAL_SURFACE ( 'NONE', #26236, 0.4848217985909654137, 0.01377952755905511792 ) ;
#13149 = DIRECTION ( 'NONE',  ( -0.000000000000000000, -1.000000000000000000, -0.000000000000000000 ) ) ;
#13150 = DIRECTION ( 'NONE',  ( 0.000000000000000000, 0.000000000000000000, 1.000000000000000000 ) ) ;
#13151 = DIRECTION ( 'NONE',  ( 1.000000000000000000, 0.000000000000000000, 0.000000000000000000 ) ) ;
#13152 = EDGE_CURVE ( 'NONE', #13674, #24360, #10962, .T. ) ;
#13153 = B_SPLINE_CURVE_WITH_KNOTS ( 'NONE', 3,
 ( #10360, #27193, #4153, #18684, #23386, #12629, #7839, #27327 ),
 .UNSPECIFIED., .F., .F.,
 ( 4, 2, 2, 4 ),
 ( 0.000000000000000000, 0.2499999999999997780, 0.4999999999999995559, 1.000000000000000000 ),
 .UNSPECIFIED. ) ;
#13154 = VERTEX_POINT ( 'NONE', #6446 ) ;
#13155 = VERTEX_POINT ( 'NONE', #15083 ) ;
#13156 = CIRCLE ( 'NONE', #993, 0.5118110236220472231 ) ;
#13157 = FACE_OUTER_BOUND ( 'NONE', #8916, .T. ) ;
#13158 = DIRECTION ( 'NONE',  ( 0.000000000000000000, 1.000000000000000000, 0.000000000000000000 ) ) ;
#13159 = CARTESIAN_POINT ( 'NONE',  ( 0.1506723201675407575, 0.000000000000000000, 0.000000000000000000 ) ) ;
#13160 = DIRECTION ( 'NONE',  ( -0.8660254037844385966, 0.4999999999999998335, 0.000000000000000000 ) ) ;
#13161 = EDGE_LOOP ( 'NONE', ( #14805, #9245, #13368, #16733, #5462 ) ) ;
#13162 = SHAPE_REPRESENTATION ( 'Output Shaft', ( #11588 ), #26943 ) ;
#13163 = CARTESIAN_POINT ( 'NONE',  ( 0.6397637795275591399, -0.7874015748031496509, 9.642888182262624280E-17 ) ) ;
#13164 = CARTESIAN_POINT ( 'NONE',  ( 0.3102399269716953345, -1.154980647406259830, -0.4411320940076480235 ) ) ;
#13165 = EDGE_CURVE ( 'NONE', #1934, #1673, #13079, .T. ) ;
#13166 = CARTESIAN_POINT ( 'NONE',  ( -0.4333973147258542991, -0.2509079296564011852, 0.2574803149606298969 ) ) ;
#13167 = DIRECTION ( 'NONE',  ( 1.000000000000000000, 0.000000000000000000, 0.000000000000000000 ) ) ;
#13168 = EDGE_LOOP ( 'NONE', ( #14160, #12613, #13302, #9424 ) ) ;
#13169 = CARTESIAN_POINT ( 'NONE',  ( 0.07874328603165660356, 0.3051025194879752878, -3.608678036488587093 ) ) ;
#13170 = FACE_OUTER_BOUND ( 'NONE', #7210, .T. ) ;
#13171 = ADVANCED_FACE ( 'NONE', ( #17050 ), #20407, .F. ) ;
#13172 = CONICAL_SURFACE ( 'NONE', #4195, 0.4537419570391968415, 1.365720138124999927 ) ;
#13173 = CARTESIAN_POINT ( 'NONE',  ( -0.1477428134820341077, 0.4351030398461640525, -1.928289503579168285 ) ) ;
#13174 = FACE_OUTER_BOUND ( 'NONE', #2081, .T. ) ;
#13175 = DIRECTION ( 'NONE',  ( 0.000000000000000000, 0.000000000000000000, 1.000000000000000000 ) ) ;
#13176 = EDGE_CURVE ( 'NONE', #88, #24094, #3931, .T. ) ;
#13177 = CARTESIAN_POINT ( 'NONE',  ( -0.5905511811023621549, -1.092519685074702762, 0.000000000000000000 ) ) ;
#13178 = CIRCLE ( 'NONE', #9121, 0.3937007874015748254 ) ;
#13179 = ORIENTED_EDGE ( 'NONE', *, *, #13927, .T. ) ;
#13180 = CARTESIAN_POINT ( 'NONE',  ( -0.2647715730835492609, -0.5498038367121063086, 0.2362204724409449064 ) ) ;
#13181 = DIRECTION ( 'NONE',  ( 0.1034422368825631960, 0.9946354626840587798, 0.000000000000000000 ) ) ;
#13182 = CARTESIAN_POINT ( 'NONE',  ( -0.3242071728275051634, -0.4225965726693019509, 1.747047244094488194 ) ) ;
#13183 = ORIENTED_EDGE ( 'NONE', *, *, #26007, .T. ) ;
#13184 = ORIENTED_EDGE ( 'NONE', *, *, #27786, .F. ) ;
#13185 = CARTESIAN_POINT ( 'NONE',  ( -0.0006737210091386627636, 0.6438792636747241449, 0.2359405056217873942 ) ) ;
#13186 = CARTESIAN_POINT ( 'NONE',  ( -0.6071195058918599230, -0.6030950601074016593, 0.9382339938617433317 ) ) ;
#13187 = CARTESIAN_POINT ( 'NONE',  ( 0.6299212598425196763, -0.07910393700787400617, 0.000000000000000000 ) ) ;
#13188 = VERTEX_POINT ( 'NONE', #5139 ) ;
#13189 = PRODUCT ( 'Index Plate', 'Index Plate', '', ( #7990 ) ) ;
#13190 = CARTESIAN_POINT ( 'NONE',  ( -0.4010740433761567081, 0.000000000000000000, -0.2480314960629921295 ) ) ;
#13191 = ORIENTED_EDGE ( 'NONE', *, *, #23596, .T. ) ;
#13192 = AXIS2_PLACEMENT_3D ( 'NONE', #3136, #9493, #22937 ) ;
#13193 = CARTESIAN_POINT ( 'NONE',  ( 0.3520466617656973218, -0.04638120790932973719, 1.953740157480315043 ) ) ;
#13194 = ORIENTED_EDGE ( 'NONE', *, *, #18637, .F. ) ;
#13195 = EDGE_CURVE ( 'NONE', #24154, #1454, #3240, .T. ) ;
#13196 = CIRCLE ( 'NONE', #11401, 0.1308464566929133932 ) ;
#13197 = LINE ( 'NONE', #21827, #17094 ) ;
#13198 = FACE_BOUND ( 'NONE', #9586, .T. ) ;
#13199 = CARTESIAN_POINT ( 'NONE',  ( -1.928513779527558736E-17, 0.000000000000000000, -0.03543307086614204404 ) ) ;
#13200 = CARTESIAN_POINT ( 'NONE',  ( -0.2602238532265429005, 0.000000000000000000, -0.07874015748031495954 ) ) ;
#13201 = EDGE_CURVE ( 'NONE', #21391, #17335, #4728, .T. ) ;
#13202 = AXIS2_PLACEMENT_3D ( 'NONE', #1579, #6253, #25597 ) ;
#13203 = EDGE_CURVE ( 'NONE', #16353, #20701, #24020, .T. ) ;
#13204 = B_SPLINE_CURVE_WITH_KNOTS ( 'NONE', 3,
 ( #1282, #7782, #18490, #5662, #1555, #27137 ),
 .UNSPECIFIED., .F., .F.,
 ( 4, 2, 4 ),
 ( 0.5000000000000000000, 0.7500000000000000000, 1.000000000000000000 ),
 .UNSPECIFIED. ) ;
#13205 = FACE_OUTER_BOUND ( 'NONE', #4216, .T. ) ;
#13206 = CARTESIAN_POINT ( 'NONE',  ( -0.3535721684717625934, 0.1200583359873131500, -3.115157480314960647 ) ) ;
#13207 = DIRECTION ( 'NONE',  ( -0.6427876096865392519, 0.7660444431189780135, 0.000000000000000000 ) ) ;
#13208 = DIRECTION ( 'NONE',  ( 0.000000000000000000, 0.000000000000000000, 1.000000000000000000 ) ) ;
#13209 = EDGE_LOOP ( 'NONE', ( #5807, #10497, #16552, #17644 ) ) ;
#13210 = CARTESIAN_POINT ( 'NONE',  ( -0.2118615749922956593, -0.5840192333899354438, 0.09685039370078740717 ) ) ;
#13211 = CIRCLE ( 'NONE', #22227, 0.6881889763779527325 ) ;
#13212 = AXIS2_PLACEMENT_3D ( 'NONE', #20785, #14299, #18504 ) ;
#13213 = ORIENTED_EDGE ( 'NONE', *, *, #22280, .F. ) ;
#13214 = ORIENTED_EDGE ( 'NONE', *, *, #3902, .T. ) ;
#13215 = FACE_OUTER_BOUND ( 'NONE', #9355, .T. ) ;
#13216 = DIRECTION ( 'NONE',  ( -1.000000000000000000, 0.000000000000000000, 0.000000000000000000 ) ) ;
#13217 = CARTESIAN_POINT ( 'NONE',  ( 0.000000000000000000, -1.707404996040164512E-16, 0.000000000000000000 ) ) ;
#13218 = VERTEX_POINT ( 'NONE', #26473 ) ;
#13219 = VERTEX_POINT ( 'NONE', #19854 ) ;
#13220 = DIRECTION ( 'NONE',  ( -0.000000000000000000, -1.000000000000000000, -0.000000000000000000 ) ) ;
#13221 = VERTEX_POINT ( 'NONE', #13210 ) ;
#13222 = CIRCLE ( 'NONE', #4653, 0.5118110236220472231 ) ;
#13223 = ORIENTED_EDGE ( 'NONE', *, *, #18285, .T. ) ;
#13225 = CARTESIAN_POINT ( 'NONE',  ( 0.3233561589689052385, -0.1867299569291582528, -3.115157480314960647 ) ) ;
#13224 = CARTESIAN_POINT ( 'NONE',  ( 0.5791695622058307125, 0.4608640948054552045, 0.2161412452810388962 ) ) ;
#13226 = ( REPRESENTATION_RELATIONSHIP ('NONE','NONE', #12434, #16232 ) REPRESENTATION_RELATIONSHIP_WITH_TRANSFORMATION ( #25269 )SHAPE_REPRESENTATION_RELATIONSHIP( ) ) ;
#13227 = CIRCLE ( 'NONE', #20449, 0.4986013261500205074 ) ;
#13228 = ORIENTED_EDGE ( 'NONE', *, *, #18680, .F. ) ;
#13229 = SPHERICAL_SURFACE ( 'NONE', #11403, 0.07677362204724409722 ) ;
#13230 = APPLICATION_CONTEXT ( 'automotive_design' ) ;
#13231 = DIRECTION ( 'NONE',  ( 0.000000000000000000, -1.000000000000000000, 0.000000000000000000 ) ) ;
#13232 = ORIENTED_EDGE ( 'NONE', *, *, #6749, .T. ) ;
#13233 = CARTESIAN_POINT ( 'NONE',  ( -0.3007905576423960392, -0.1482986320106512990, 1.953740157480315043 ) ) ;
#13234 = ORIENTED_EDGE ( 'NONE', *, *, #19361, .T. ) ;
#13235 = VERTEX_POINT ( 'NONE', #17850 ) ;
#13236 = DIRECTION ( 'NONE',  ( 0.000000000000000000, -1.000000000000000000, 0.000000000000000000 ) ) ;
#13237 = VERTEX_POINT ( 'NONE', #6865 ) ;
#13238 = ORIENTED_EDGE ( 'NONE', *, *, #25655, .F. ) ;
#13239 = ORIENTED_EDGE ( 'NONE', *, *, #18218, .T. ) ;
#13240 = DIRECTION ( 'NONE',  ( 0.000000000000000000, 1.000000000000000000, 0.000000000000000000 ) ) ;
#13241 = EDGE_CURVE ( 'NONE', #19022, #18692, #6888, .T. ) ;
#13242 = CIRCLE ( 'NONE', #7367, 0.5905511811200284678 ) ;
#13243 = TOROIDAL_SURFACE ( 'NONE', #1072, 0.3031496062992122820, 0.01181102362204755792 ) ;
#13245 = FACE_BOUND ( 'NONE', #19302, .T. ) ;
#13246 = CARTESIAN_POINT ( 'NONE',  ( -0.08582672153403875237, 0.3030863606044028602, -3.598133626470924273 ) ) ;
#13247 = CARTESIAN_POINT ( 'NONE',  ( 0.7864367829959311162, 0.4380964431885162602, 0.1600151387865518249 ) ) ;
#13248 = ORIENTED_EDGE ( 'NONE', *, *, #11726, .F. ) ;
#13249 = AXIS2_PLACEMENT_3D ( 'NONE', #20902, #1547, #27405 ) ;
#13250 = CARTESIAN_POINT ( 'NONE',  ( 0.6055690743987126590, 0.5162970762339605946, 0.000000000000000000 ) ) ;
#13251 = ITEM_DEFINED_TRANSFORMATION ( 'NONE', 'NONE', #2144,  #11588 ) ;
#13252 = AXIS2_PLACEMENT_3D ( 'NONE', #27367, #14382, #12386 ) ;
#13253 = CARTESIAN_POINT ( 'NONE',  ( -0.5664154050804837137, 1.115659691807800558, 0.04720470158372228747 ) ) ;
#13254 = CARTESIAN_POINT ( 'NONE',  ( 0.000000000000000000, 0.000000000000000000, -0.2204724409448818867 ) ) ;
#13255 = DIRECTION ( 'NONE',  ( -1.000000000000000000, 0.000000000000000000, 0.000000000000000000 ) ) ;
#13256 = CARTESIAN_POINT ( 'NONE',  ( -0.8725268807032540153, 0.000000000000000000, -1.052618110236220428 ) ) ;
#13257 = EDGE_CURVE ( 'NONE', #2437, #6891, #18596, .T. ) ;
#13258 = DIRECTION ( 'NONE',  ( 0.000000000000000000, 1.000000000000000000, 0.000000000000000000 ) ) ;
#13259 = ADVANCED_FACE ( 'NONE', ( #8969 ), #5548, .T. ) ;
#13260 = B_SPLINE_CURVE_WITH_KNOTS ( 'NONE', 3,
 ( #9627, #27298, #9917, #27023, #23072, #5258 ),
 .UNSPECIFIED., .F., .F.,
 ( 4, 2, 4 ),
 ( 1.162880698919837918, 1.164573402063409979, 1.166266105206986037 ),
 .UNSPECIFIED. ) ;
#13261 = CARTESIAN_POINT ( 'NONE',  ( -0.8725268807032540153, 0.000000000000000000, -1.052618110236220428 ) ) ;
#13262 = ORIENTED_EDGE ( 'NONE', *, *, #8372, .F. ) ;
#13263 = PRODUCT_RELATED_PRODUCT_CATEGORY ( 'part', '', ( #10231 ) ) ;
#13264 = CARTESIAN_POINT ( 'NONE',  ( -1.692913385826771533, 0.4724409448818898127, -1.036610629921259805E-16 ) ) ;
#13265 = ( CONVERSION_BASED_UNIT ( 'INCH', #4638 ) LENGTH_UNIT ( ) NAMED_UNIT ( #6740 ) ) ;
#13266 = DIRECTION ( 'NONE',  ( -1.000000000000000000, 0.000000000000000000, 0.000000000000000000 ) ) ;
#13267 = ORIENTED_EDGE ( 'NONE', *, *, #21916, .F. ) ;
#13268 = FACE_OUTER_BOUND ( 'NONE', #14514, .T. ) ;
#13269 = CIRCLE ( 'NONE', #14652, 0.4247824285122252519 ) ;
#13270 = CARTESIAN_POINT ( 'NONE',  ( -0.4921259842519685179, 0.000000000000000000, -1.569881889763779625 ) ) ;
#13271 = FACE_OUTER_BOUND ( 'NONE', #21293, .T. ) ;
#13272 = ADVANCED_FACE ( 'NONE', ( #13482, #7134 ), #9102, .T. ) ;
#13273 = CARTESIAN_POINT ( 'NONE',  ( -0.3665264996331779601, -0.2116141732283464416, 0.2145688976377952695 ) ) ;
#13274 = CIRCLE ( 'NONE', #10567, 0.3771653543307086909 ) ;
#13275 = ORIENTED_EDGE ( 'NONE', *, *, #19557, .F. ) ;
#13276 = CARTESIAN_POINT ( 'NONE',  ( -0.2442565704126240245, -0.4954197419817664150, 0.9202755905511811330 ) ) ;
#13277 = DIRECTION ( 'NONE',  ( -0.000000000000000000, -1.000000000000000000, -0.000000000000000000 ) ) ;
#13278 = ORIENTED_EDGE ( 'NONE', *, *, #8377, .F. ) ;
#13279 = DIRECTION ( 'NONE',  ( 0.000000000000000000, 0.000000000000000000, 1.000000000000000000 ) ) ;
#13280 = CARTESIAN_POINT ( 'NONE',  ( 0.1704479274140477119, -0.4700505334956465164, 0.1496602734632995202 ) ) ;
#13281 = DIRECTION ( 'NONE',  ( -0.000000000000000000, -1.000000000000000000, -0.000000000000000000 ) ) ;
#13282 = FACE_OUTER_BOUND ( 'NONE', #7993, .T. ) ;
#13283 = CARTESIAN_POINT ( 'NONE',  ( 0.000000000000000000, 0.000000000000000000, 0.2574803149606298969 ) ) ;
#13284 = VECTOR ( 'NONE', #18917, 39.37007874015748143 ) ;
#13285 = CARTESIAN_POINT ( 'NONE',  ( -0.07870736599818195511, 0.2165354330708661457, -3.608715228723579305 ) ) ;
#13286 = ( BOUNDED_CURVE ( )  B_SPLINE_CURVE ( 2, ( #5342, #10839, #23439 ),
 .UNSPECIFIED., .F., .T. ) 
 B_SPLINE_CURVE_WITH_KNOTS ( ( 3, 3 ),
 ( 0.1168436138077912356, 0.2336872276155829986 ),
 .UNSPECIFIED. ) 
 CURVE ( )  GEOMETRIC_REPRESENTATION_ITEM ( )  RATIONAL_B_SPLINE_CURVE ( ( 1.077350269189625953, 1.077350269189626175, 1.000000000000000000 ) ) 
 REPRESENTATION_ITEM ( '' )  ) ;
#13287 = DIRECTION ( 'NONE',  ( 0.000000000000000000, 0.000000000000000000, 1.000000000000000000 ) ) ;
#13288 = CARTESIAN_POINT ( 'NONE',  ( 0.03425350366399289304, 0.07114503267349270299, -0.4653551329966305605 ) ) ;
#13289 = CARTESIAN_POINT ( 'NONE',  ( 0.000000000000000000, 0.000000000000000000, -0.04133858267716535029 ) ) ;
#13290 = EDGE_LOOP ( 'NONE', ( #9725, #1530, #25757 ) ) ;
#13291 = DIRECTION ( 'NONE',  ( -0.000000000000000000, 1.000000000000000000, -0.000000000000000000 ) ) ;
#13292 = TOROIDAL_SURFACE ( 'NONE', #242, 0.6102362204724409711, 0.1299212598425196763 ) ;
#13293 = ADVANCED_FACE ( 'NONE', ( #22385 ), #21349, .T. ) ;
#13294 = CARTESIAN_POINT ( 'NONE',  ( 0.5417097841048533757, -0.1839420097223136985, 0.9399606299212598381 ) ) ;
#13295 = CARTESIAN_POINT ( 'NONE',  ( 0.000000000000000000, 0.000000000000000000, 0.1771653543307086520 ) ) ;
#13296 = ORIENTED_EDGE ( 'NONE', *, *, #17460, .F. ) ;
#13297 = CARTESIAN_POINT ( 'NONE',  ( -0.5021077788565687650, -0.1139291307084100563, 0.3251195115539141645 ) ) ;
#13298 = ORIENTED_EDGE ( 'NONE', *, *, #26914, .T. ) ;
#13299 = ADVANCED_FACE ( 'NONE', ( #22110 ), #15023, .T. ) ;
#13300 = EDGE_CURVE ( 'NONE', #11508, #25524, #12300, .T. ) ;
#13301 = VECTOR ( 'NONE', #6737, 39.37007874015748143 ) ;
#13302 = ORIENTED_EDGE ( 'NONE', *, *, #19376, .T. ) ;
#13303 = DIRECTION ( 'NONE',  ( -0.9575713608335526539, 0.1440981340193014382, 0.2495852893972990150 ) ) ;
#13304 = EDGE_CURVE ( 'NONE', #8484, #18347, #170, .T. ) ;
#13305 = CARTESIAN_POINT ( 'NONE',  ( 0.4621951630817676682, 0.08130208312401811244, 0.07637549214372854611 ) ) ;
#13306 = CARTESIAN_POINT ( 'NONE',  ( -0.6299212598425196763, 0.9448818897637796255, -9.561468503937007847E-18 ) ) ;
#13307 = ORIENTED_EDGE ( 'NONE', *, *, #7084, .F. ) ;
#13308 = CARTESIAN_POINT ( 'NONE',  ( -0.2997912780622380979, -0.1736589463928937815, 0.1377952755905510751 ) ) ;
#13309 = DIRECTION ( 'NONE',  ( 0.000000000000000000, 0.000000000000000000, -1.000000000000000000 ) ) ;
#13310 = AXIS2_PLACEMENT_3D ( 'NONE', #199, #1993, #8768 ) ;
#13311 = DIRECTION ( 'NONE',  ( 0.000000000000000000, -7.180547322999999937E-06, -0.9999999999742198442 ) ) ;
#13312 = CARTESIAN_POINT ( 'NONE',  ( 0.1180276236025431108, -0.3257325899126714552, 0.1377952755905513527 ) ) ;
#13313 = DIRECTION ( 'NONE',  ( 0.000000000000000000, 0.000000000000000000, 1.000000000000000000 ) ) ;
#13314 = PLANE ( 'NONE',  #11848 ) ;
#13315 = ORIENTED_EDGE ( 'NONE', *, *, #9549, .F. ) ;
#13316 = LINE ( 'NONE', #229, #2182 ) ;
#13317 = CARTESIAN_POINT ( 'NONE',  ( -0.1585706980422252055, -0.4669911931914896841, -1.569881889763779625 ) ) ;
#13318 = AXIS2_PLACEMENT_3D ( 'NONE', #5630, #1523, #3341 ) ;
#13319 = CARTESIAN_POINT ( 'NONE',  ( 0.000000000000000000, 0.000000000000000000, 0.1322834645669291320 ) ) ;
#13320 = CARTESIAN_POINT ( 'NONE',  ( 0.1477428134820237549, -0.4351030398461813720, -1.928289503579156294 ) ) ;
#13321 = CARTESIAN_POINT ( 'NONE',  ( -0.5335524835332333682, 0.1429116519061236767, 0.9202755905511811330 ) ) ;
#13322 = CARTESIAN_POINT ( 'NONE',  ( -0.5385210225480960844, 0.4284847435812472183, 0.3401574803149606252 ) ) ;
#13323 = CARTESIAN_POINT ( 'NONE',  ( -0.5501272683015652198, 0.4396946356883123519, 0.3281099440159496172 ) ) ;
#13325 = ADVANCED_FACE ( 'NONE', ( #19817 ), #479, .T. ) ;
#13324 = AXIS2_PLACEMENT_3D ( 'NONE', #5264, #11758, #22504 ) ;
#13326 = CARTESIAN_POINT ( 'NONE',  ( 2.664928230027803213, 0.9448818897637796255, 0.1082677165354330451 ) ) ;
#13327 = CIRCLE ( 'NONE', #22339, 0.1003956692913385851 ) ;
#13328 = CARTESIAN_POINT ( 'NONE',  ( -0.6505662911506299162, -0.01296944263642094489, -0.2362868447687200835 ) ) ;
#13329 = SPHERICAL_SURFACE ( 'NONE', #13601, 0.1299232283464566984 ) ;
#13330 = EDGE_CURVE ( 'NONE', #10350, #25, #14031, .T. ) ;
#13331 = DIRECTION ( 'NONE',  ( 0.7071067818211385081, -0.7071067805519564153, 0.000000000000000000 ) ) ;
#13332 = ORIENTED_EDGE ( 'NONE', *, *, #11814, .F. ) ;
#13333 = AXIS2_PLACEMENT_3D ( 'NONE', #20837, #2044, #1488 ) ;
#13334 = CARTESIAN_POINT ( 'NONE',  ( 0.000000000000000000, 0.000000000000000000, 0.3401574803149606252 ) ) ;
#13335 = CARTESIAN_POINT ( 'NONE',  ( 0.000000000000000000, 0.000000000000000000, -0.1377952755696461029 ) ) ;
#13336 = CARTESIAN_POINT ( 'NONE',  ( 0.4164331889188472857, 0.3315254675241992577, 0.3401591244667909186 ) ) ;
#13337 = AXIS2_PLACEMENT_3D ( 'NONE', #13334, #11207, #19829 ) ;
#13338 = ORIENTED_EDGE ( 'NONE', *, *, #6493, .T. ) ;
#13339 = CARTESIAN_POINT ( 'NONE',  ( -0.0005189969344232283309, 0.3771649972486724733, 0.1992125984251968684 ) ) ;
#13340 = ORIENTED_EDGE ( 'NONE', *, *, #1685, .T. ) ;
#13341 = CARTESIAN_POINT ( 'NONE',  ( 0.1516263115863346334, 0.1971492568089271424, -0.4530651079966795947 ) ) ;
#13342 = CARTESIAN_POINT ( 'NONE',  ( 0.0005855335178282750032, 0.4865383137623722209, 0.1075369453635709044 ) ) ;
#13343 = EDGE_CURVE ( 'NONE', #1560, #11010, #24133, .T. ) ;
#13344 = FACE_BOUND ( 'NONE', #9898, .T. ) ;
#13345 = CARTESIAN_POINT ( 'NONE',  ( -0.2836590635674538508, 0.2488091035917008864, -3.100567304031763172 ) ) ;
#13346 = TOROIDAL_SURFACE ( 'NONE', #25981, 0.5610236220472440971, 0.1003937007874015908 ) ;
#13347 = DIRECTION ( 'NONE',  ( 0.000000000000000000, 1.000000000000000000, 0.000000000000000000 ) ) ;
#13348 = CARTESIAN_POINT ( 'NONE',  ( -0.05118110236220472370, 0.5935039370078740717, 0.000000000000000000 ) ) ;
#13349 = DIRECTION ( 'NONE',  ( -0.000000000000000000, 1.000000000000000000, -0.000000000000000000 ) ) ;
#13350 = VERTEX_POINT ( 'NONE', #13727 ) ;
#13351 = CARTESIAN_POINT ( 'NONE',  ( -0.4446020952038907681, 0.02909913904661337244, -1.934055118110236338 ) ) ;
#13352 = CIRCLE ( 'NONE', #716, 0.3937007873768824662 ) ;
#13353 = ADVANCED_FACE ( 'NONE', ( #7515 ), #14304, .F. ) ;
#13354 = ORIENTED_EDGE ( 'NONE', *, *, #3968, .T. ) ;
#13355 = LINE ( 'NONE', #9376, #13301 ) ;
#13356 = CARTESIAN_POINT ( 'NONE',  ( 0.5118110236220472231, 3.133938659235352953E-17, 1.766732283464566899 ) ) ;
#13357 = CARTESIAN_POINT ( 'NONE',  ( -0.4069448477556027455, 0.3121994997598392940, 1.747047244094488194 ) ) ;
#13358 = EDGE_CURVE ( 'NONE', #25578, #17014, #9972, .T. ) ;
#13359 = DIRECTION ( 'NONE',  ( 0.000000000000000000, 0.000000000000000000, -1.000000000000000000 ) ) ;
#13360 = ORIENTED_EDGE ( 'NONE', *, *, #6046, .F. ) ;
#13361 = ORIENTED_EDGE ( 'NONE', *, *, #2175, .F. ) ;
#13363 = CARTESIAN_POINT ( 'NONE',  ( -0.3349073414798397486, -0.1651192144506304638, -3.115157480314960647 ) ) ;
#13362 = CARTESIAN_POINT ( 'NONE',  ( 0.5754648248631183405, 0.4579130143391036412, 0.2763636194408833902 ) ) ;
#13364 = ORIENTED_EDGE ( 'NONE', *, *, #22350, .F. ) ;
#13365 = CARTESIAN_POINT ( 'NONE',  ( 0.1532705055535415473, -0.5147072688414000563, -0.4165008336377047371 ) ) ;
#13366 = DIRECTION ( 'NONE',  ( 0.000000000000000000, 1.000000000000000000, 0.000000000000000000 ) ) ;
#13367 = ORIENTED_EDGE ( 'NONE', *, *, #25098, .F. ) ;
#13368 = ORIENTED_EDGE ( 'NONE', *, *, #12759, .F. ) ;
#13369 = CONICAL_SURFACE ( 'NONE', #2964, 0.4526932812344527379, 0.1178097243749990780 ) ;
#13370 = EDGE_CURVE ( 'NONE', #10570, #12770, #16362, .T. ) ;
#13371 = FACE_OUTER_BOUND ( 'NONE', #16982, .T. ) ;
#13372 = ORIENTED_EDGE ( 'NONE', *, *, #18017, .T. ) ;
#13373 = CARTESIAN_POINT ( 'NONE',  ( -1.197070535079588716, 0.07874015748031495954, 1.197070535079588716 ) ) ;
#13374 = CARTESIAN_POINT ( 'NONE',  ( -0.2268956277328164628, -0.4599954779396636662, -1.550196850393700920 ) ) ;
#13375 = ORIENTED_EDGE ( 'NONE', *, *, #8711, .T. ) ;
#13376 = ORIENTED_EDGE ( 'NONE', *, *, #3005, .F. ) ;
#13377 = B_SPLINE_CURVE_WITH_KNOTS ( 'NONE', 3,
 ( #4468, #10680, #17321, #25939, #23696, #6592 ),
 .UNSPECIFIED., .F., .F.,
 ( 4, 2, 4 ),
 ( 0.9359046326925629655, 0.9375808709372039917, 0.9392571091818440188 ),
 .UNSPECIFIED. ) ;
#13378 = ADVANCED_FACE ( 'NONE', ( #18654 ), #14124, .F. ) ;
#13379 = DIRECTION ( 'NONE',  ( 1.000000000000000000, 0.000000000000000000, 0.000000000000000000 ) ) ;
#13380 = CARTESIAN_POINT ( 'NONE',  ( -0.06294381634922237290, 0.1968503937007874127, -3.224230184698364976 ) ) ;
#13381 = CARTESIAN_POINT ( 'NONE',  ( 0.7529539909399990405, 0.6316670891464889470, 0.07132544462029670462 ) ) ;
#13382 = ORIENTED_EDGE ( 'NONE', *, *, #1096, .F. ) ;
#13383 = DIRECTION ( 'NONE',  ( 0.000000000000000000, 1.000000000000000000, 0.000000000000000000 ) ) ;
#13384 = VECTOR ( 'NONE', #6474, 39.37007874015748143 ) ;
#13385 = CARTESIAN_POINT ( 'NONE',  ( 0.000000000000000000, 0.000000000000000000, 0.1377952755905511861 ) ) ;
#13386 = AXIS2_PLACEMENT_3D ( 'NONE', #11016, #11289, #8755 ) ;
#13387 = CARTESIAN_POINT ( 'NONE',  ( -0.3666422121843372350, -1.088756306996242484, -0.3628375440173792765 ) ) ;
#13388 = CARTESIAN_POINT ( 'NONE',  ( -0.03425350366399289304, -0.07114503267349270299, -0.4653551329966305605 ) ) ;
#13389 = CARTESIAN_POINT ( 'NONE',  ( 0.000000000000000000, 0.000000000000000000, 2.504921259842519898 ) ) ;
#13390 = DIRECTION ( 'NONE',  ( 0.000000000000000000, 1.000000000000000000, 0.000000000000000000 ) ) ;
#13391 = EDGE_CURVE ( 'NONE', #19933, #19454, #20075, .T. ) ;
#13392 = ( NAMED_UNIT ( * ) SI_UNIT ( $, .STERADIAN. ) SOLID_ANGLE_UNIT ( ) ) ;
#13393 = B_SPLINE_CURVE_WITH_KNOTS ( 'NONE', 3,
 ( #10868, #21890, #21752, #11012, #310, #8884, #19764, #17504, #15414, #4639, #431, #15541, #9278, #20036, #7183, #13671, #22291, #14510, #974, #23111, #26663, #27486, #8134, #23257, #11695, #20316, #16088, #13969, #25641, #21540, #17164, #15194, #23806, #13059 ),
 .UNSPECIFIED., .F., .F.,
 ( 4, 2, 2, 2, 2, 2, 2, 2, 2, 2, 2, 2, 2, 2, 2, 2, 4 ),
 ( 0.000000000000000000, 0.03125000000000000000, 0.06250000000000000000, 0.09375000000000000000, 0.1250000000000000000, 0.1562500000000000000, 0.1875000000000000000, 0.2187500000000000278, 0.2500000000000000555, 0.2812500000000000555, 0.3125000000000000555, 0.3437500000000000555, 0.3750000000000000555, 0.4062500000000000555, 0.4375000000000000555, 0.4687500000000000555, 0.5000000000000000000 ),
 .UNSPECIFIED. ) ;
#13394 = CARTESIAN_POINT ( 'NONE',  ( -0.07874015748031502893, 0.1968503937007873850, -3.272637795275590733 ) ) ;
#13395 = EDGE_LOOP ( 'NONE', ( #10685, #8445, #13022, #4889, #11908, #18849 ) ) ;
#13396 = DIRECTION ( 'NONE',  ( -1.000000000000000000, 0.000000000000000000, 0.000000000000000000 ) ) ;
#13397 = CARTESIAN_POINT ( 'NONE',  ( 0.000000000000000000, 0.000000000000000000, 0.6299212598425196763 ) ) ;
#13398 = ORIENTED_EDGE ( 'NONE', *, *, #13508, .F. ) ;
#13399 = FACE_BOUND ( 'NONE', #80, .T. ) ;
#13400 = CARTESIAN_POINT ( 'NONE',  ( 0.000000000000000000, 0.000000000000000000, 0.2755905511811023723 ) ) ;
#13401 = ORIENTED_EDGE ( 'NONE', *, *, #1538, .T. ) ;
#13402 = CARTESIAN_POINT ( 'NONE',  ( -0.4783323773986625782, 0.2762247810518428381, 0.9399606299212598381 ) ) ;
#13403 = DIMENSIONAL_EXPONENTS ( 1.000000000000000000, 0.000000000000000000, 0.000000000000000000, 0.000000000000000000, 0.000000000000000000, 0.000000000000000000, 0.000000000000000000 ) ;
#13404 = ORIENTED_EDGE ( 'NONE', *, *, #19269, .F. ) ;
#13405 = CARTESIAN_POINT ( 'NONE',  ( 0.000000000000000000, 0.09092130223458683158, -0.3779527559055118058 ) ) ;
#13406 = ORIENTED_EDGE ( 'NONE', *, *, #6155, .F. ) ;
#13407 = CARTESIAN_POINT ( 'NONE',  ( -7.279147705782180972E-18, 0.5322834645669292097, 0.1322810039474933141 ) ) ;
#13408 = DIRECTION ( 'NONE',  ( 0.000000000000000000, 0.000000000000000000, -1.000000000000000000 ) ) ;
#13409 = CARTESIAN_POINT ( 'NONE',  ( 0.03008364706454716778, -0.1136516277932334562, 0.1968503937007874127 ) ) ;
#13410 = DIRECTION ( 'NONE',  ( -1.000000000000000000, 0.000000000000000000, 0.000000000000000000 ) ) ;
#13411 = CARTESIAN_POINT ( 'NONE',  ( -0.3992017438595018564, -0.2298214351608254269, 0.1771653543307087630 ) ) ;
#13412 = EDGE_CURVE ( 'NONE', #17502, #22837, #21783, .T. ) ;
#13413 = DIRECTION ( 'NONE',  ( 0.000000000000000000, 0.000000000000000000, -1.000000000000000000 ) ) ;
#13414 = AXIS2_PLACEMENT_3D ( 'NONE', #17411, #8656, #17279 ) ;
#13415 = CARTESIAN_POINT ( 'NONE',  ( 6.557635703933409897E-17, 0.3771653543307084688, 0.07637549214372833795 ) ) ;
#13416 = CARTESIAN_POINT ( 'NONE',  ( -0.3132247436399438478, 0.3723693495123709396, 0.1827409795197761921 ) ) ;
#13417 = CARTESIAN_POINT ( 'NONE',  ( 0.4300830224589218820, 0.3772436174784425389, 0.9399606299212598381 ) ) ;
#13418 = CARTESIAN_POINT ( 'NONE',  ( 0.5118110236220472231, 3.133938659235352953E-17, 1.766732283464566899 ) ) ;
#13419 = EDGE_CURVE ( 'NONE', #6563, #14294, #18133, .T. ) ;
#13420 = MECHANICAL_DESIGN_GEOMETRIC_PRESENTATION_REPRESENTATION (  '', ( #3013 ), #2145 ) ;
#13421 = CARTESIAN_POINT ( 'NONE',  ( -2.685748425196850164E-17, 0.000000000000000000, -3.745078740157480546 ) ) ;
#13422 = PRODUCT_DEFINITION_SHAPE ( 'NONE', 'NONE',  #27923 ) ;
#13423 = CARTESIAN_POINT ( 'NONE',  ( 9.642888182478974314E-17, 0.1968503937007875237, 0.7874015748208159637 ) ) ;
#13424 = CARTESIAN_POINT ( 'NONE',  ( -0.5096726623812283252, -0.1170085733290669172, 0.1392975274269444008 ) ) ;
#13425 = ORIENTED_EDGE ( 'NONE', *, *, #15906, .F. ) ;
#13426 = CARTESIAN_POINT ( 'NONE',  ( 0.000000000000000000, 0.000000000000000000, -0.1309055118110236116 ) ) ;
#13427 = CARTESIAN_POINT ( 'NONE',  ( 0.1516263115863346334, -0.2937912646890007973, -0.3972688187320929099 ) ) ;
#13428 = VERTEX_POINT ( 'NONE', #20513 ) ;
#13429 = FACE_OUTER_BOUND ( 'NONE', #25801, .T. ) ;
#13430 = ORIENTED_EDGE ( 'NONE', *, *, #8614, .F. ) ;
#13431 = CIRCLE ( 'NONE', #10750, 0.09842519685039370636 ) ;
#13432 = LINE ( 'NONE', #2558, #25233 ) ;
#13433 = ADVANCED_FACE ( 'NONE', ( #9769 ), #6007, .T. ) ;
#13434 = VECTOR ( 'NONE', #5328, 39.37007874015748143 ) ;
#13435 = CARTESIAN_POINT ( 'NONE',  ( -0.6117448998508523417, 0.1083144418130960601, 0.09684874924366436433 ) ) ;
#13436 = CARTESIAN_POINT ( 'NONE',  ( 0.7430739993161732393, 0.7025059129074271436, 0.04061420537818291598 ) ) ;
#13437 = DIRECTION ( 'NONE',  ( 0.000000000000000000, 0.000000000000000000, 1.000000000000000000 ) ) ;
#13438 = ADVANCED_FACE ( 'NONE', ( #8089 ), #5069, .F. ) ;
#13439 = CARTESIAN_POINT ( 'NONE',  ( -0.04593175845765267579, -4.927204724409449161E-18, 0.000000000000000000 ) ) ;
#13440 = CARTESIAN_POINT ( 'NONE',  ( -0.01968503937007873988, 0.6102362204724409711, -7.473238341253533632E-17 ) ) ;
#13441 = CARTESIAN_POINT ( 'NONE',  ( -0.3665264996331779601, -0.2116141732283464416, 0.1377952755905511861 ) ) ;
#13442 = VERTEX_POINT ( 'NONE', #12733 ) ;
#13443 = AXIS2_PLACEMENT_3D ( 'NONE', #25005, #14737, #5669 ) ;
#13444 = DIRECTION ( 'NONE',  ( 1.000000000000000000, -1.147443000000000016E-15, 0.000000000000000000 ) ) ;
#13445 = CARTESIAN_POINT ( 'NONE',  ( -0.2466292688015021273, -0.4270824798167794922, -1.550196850393700920 ) ) ;
#13446 = EDGE_CURVE ( 'NONE', #19463, #18018, #19077, .T. ) ;
#13447 = CARTESIAN_POINT ( 'NONE',  ( 0.4438564651657277427, 0.1188866373884867045, -1.928289503579172726 ) ) ;
#13448 = CARTESIAN_POINT ( 'NONE',  ( -0.1429116519061127688, 0.5335524835332354776, 0.9202755905511811330 ) ) ;
#13449 = ORIENTED_EDGE ( 'NONE', *, *, #15648, .T. ) ;
#13450 = FACE_OUTER_BOUND ( 'NONE', #175, .T. ) ;
#13451 = EDGE_CURVE ( 'NONE', #20543, #4605, #10038, .T. ) ;
#13452 = CARTESIAN_POINT ( 'NONE',  ( -0.4688657571743239938, 0.08326155277091105977, 0.2330651857748314848 ) ) ;
#13453 = CARTESIAN_POINT ( 'NONE',  ( -0.2297883689023087483, 0.3979194638820583441, -1.928289503579160513 ) ) ;
#13454 = AXIS2_PLACEMENT_3D ( 'NONE', #9708, #20867, #3194 ) ;
#13455 = AXIS2_PLACEMENT_3D ( 'NONE', #12490, #21108, #10639 ) ;
#13456 = CARTESIAN_POINT ( 'NONE',  ( -0.6208708315385689236, -0.09594997026702008214, -0.08344808172604054053 ) ) ;
#13457 = CARTESIAN_POINT ( 'NONE',  ( -0.2362204724409449064, 0.000000000000000000, 0.000000000000000000 ) ) ;
#13458 = CARTESIAN_POINT ( 'NONE',  ( 1.692913385826771533, 0.4724409448818898127, 3.109831496062992451E-16 ) ) ;
#13459 = CARTESIAN_POINT ( 'NONE',  ( 0.07614184848677874040, 0.000000000000000000, 0.000000000000000000 ) ) ;
#13461 = DIRECTION ( 'NONE',  ( -1.000000000000000000, 0.000000000000000000, 0.000000000000000000 ) ) ;
#13460 = TOROIDAL_SURFACE ( 'NONE', #19348, 0.4980314960629921295, 0.01377952755905511792 ) ;
#13462 = CYLINDRICAL_SURFACE ( 'NONE', #18121, 0.7283464566929134243 ) ;
#13463 = B_SPLINE_CURVE_WITH_KNOTS ( 'NONE', 3,
 ( #25594, #23492, #12728, #10892, #21356, #19507 ),
 .UNSPECIFIED., .F., .F.,
 ( 4, 2, 4 ),
 ( 0.000000000000000000, 0.2500000000000000000, 0.5000000000000000000 ),
 .UNSPECIFIED. ) ;
#13464 = ORIENTED_EDGE ( 'NONE', *, *, #2564, .F. ) ;
#13465 = CARTESIAN_POINT ( 'NONE',  ( -0.6587140840999922142, 0.005767656754036574844, -0.2362204724409449064 ) ) ;
#13466 = ORIENTED_EDGE ( 'NONE', *, *, #8797, .F. ) ;
#13467 = DIRECTION ( 'NONE',  ( 1.000000000000000000, 0.000000000000000000, 0.000000000000000000 ) ) ;
#13468 = LINE ( 'NONE', #10812, #17446 ) ;
#13469 = DIRECTION ( 'NONE',  ( 0.000000000000000000, 1.224646799147353207E-16, 1.000000000000000000 ) ) ;
#13470 = CIRCLE ( 'NONE', #1310, 2.066929133858267598 ) ;
#13471 = EDGE_CURVE ( 'NONE', #15836, #5312, #8616, .T. ) ;
#13472 = CIRCLE ( 'NONE', #18447, 0.8267716535433071723 ) ;
#13473 = CARTESIAN_POINT ( 'NONE',  ( 0.02917857698710651232, -0.4446006764000813294, -1.934055118110236338 ) ) ;
#13474 = CARTESIAN_POINT ( 'NONE',  ( -0.1886891683788859964, 0.3267488823401775155, -3.100567304031764948 ) ) ;
#13475 = AXIS2_PLACEMENT_3D ( 'NONE', #2442, #23933, #6189 ) ;
#13476 = DIRECTION ( 'NONE',  ( 1.000000000000000000, 0.000000000000000000, 0.000000000000000000 ) ) ;
#13477 = CARTESIAN_POINT ( 'NONE',  ( 0.3223547283257516272, 0.3832433309296771617, 0.09685039370078740717 ) ) ;
#13478 = CARTESIAN_POINT ( 'NONE',  ( 0.1504366439317611215, 0.2749075979901894895, 0.3999374451793131779 ) ) ;
#13479 = B_SPLINE_CURVE_WITH_KNOTS ( 'NONE', 3,
 ( #4828, #22067, #19949, #2698, #15332, #23929, #4563, #13169, #21801, #20511, #5099, #17938, #11470, #9619 ),
 .UNSPECIFIED., .F., .F.,
 ( 4, 2, 2, 2, 2, 2, 4 ),
 ( -0.002956005455613042350, -0.002463754750849624520, -0.001971504046086206691, -0.0009870026365593714650, -2.501227032536239292E-06, 0.0004897494777309002387, 0.0009820001824943367166 ),
 .UNSPECIFIED. ) ;
#13480 = ADVANCED_FACE ( 'NONE', ( #18799 ), #3728, .T. ) ;
#13481 = EDGE_LOOP ( 'NONE', ( #23542, #2898 ) ) ;
#13482 = FACE_BOUND ( 'NONE', #6780, .T. ) ;
#13483 = CARTESIAN_POINT ( 'NONE',  ( -0.4438564651657384008, -0.1188866373884874261, -1.928289503579162067 ) ) ;
#13484 = CARTESIAN_POINT ( 'NONE',  ( 0.4465874321618643061, 0.1200170377978878322, -1.928289503579156516 ) ) ;
#13485 = EDGE_LOOP ( 'NONE', ( #23366, #11916 ) ) ;
#13486 = CARTESIAN_POINT ( 'NONE',  ( 0.1198326771653543399, 0.000000000000000000, 0.000000000000000000 ) ) ;
#13487 = DIRECTION ( 'NONE',  ( 0.000000000000000000, 0.000000000000000000, 1.000000000000000000 ) ) ;
#13488 = SHAPE_DEFINITION_REPRESENTATION ( #16330, #1615 ) ;
#13489 = CARTESIAN_POINT ( 'NONE',  ( -0.3382184156732160329, -0.3855916753051698009, 1.747047244094488194 ) ) ;
#13490 = VERTEX_POINT ( 'NONE', #14457 ) ;
#13491 = CARTESIAN_POINT ( 'NONE',  ( 0.3607825703598260825, 0.06309631803675713746, 0.1910323753036465011 ) ) ;
#13492 = EDGE_CURVE ( 'NONE', #17206, #17635, #9580, .T. ) ;
#13493 = ORIENTED_EDGE ( 'NONE', *, *, #4541, .F. ) ;
#13494 = AXIS2_PLACEMENT_3D ( 'NONE', #21000, #4191, #1216 ) ;
#13495 = CARTESIAN_POINT ( 'NONE',  ( 0.2462256503455907131, -0.2807137536170764003, -3.115157480314960647 ) ) ;
#13496 = DIRECTION ( 'NONE',  ( -1.000000000000000000, 0.000000000000000000, 0.000000000000000000 ) ) ;
#13497 = CARTESIAN_POINT ( 'NONE',  ( 0.1755067523729419432, -0.6057501678605275997, 7.418299212598425247E-17 ) ) ;
#13498 = CARTESIAN_POINT ( 'NONE',  ( 0.1482986320106464417, 0.3007905576423925420, 1.953740157480315043 ) ) ;
#13499 = EDGE_LOOP ( 'NONE', ( #686, #16710, #19083, #26892 ) ) ;
#13500 = EDGE_LOOP ( 'NONE', ( #11557, #17054, #19385, #6074, #21023 ) ) ;
#13501 = ORIENTED_EDGE ( 'NONE', *, *, #23784, .T. ) ;
#13502 = ORIENTED_EDGE ( 'NONE', *, *, #544, .F. ) ;
#13503 = VERTEX_POINT ( 'NONE', #8633 ) ;
#13504 = ORIENTED_EDGE ( 'NONE', *, *, #8464, .F. ) ;
#13505 = VERTEX_POINT ( 'NONE', #23067 ) ;
#13506 = DIRECTION ( 'NONE',  ( 0.000000000000000000, -1.000000000000000000, 0.000000000000000000 ) ) ;
#13507 = ADVANCED_FACE ( 'NONE', ( #8371 ), #3684, .T. ) ;
#13508 = EDGE_CURVE ( 'NONE', #19742, #19722, #7792, .T. ) ;
#13509 = FACE_OUTER_BOUND ( 'NONE', #6400, .T. ) ;
#13510 = CARTESIAN_POINT ( 'NONE',  ( -0.5118110236220473341, 0.000000000000000000, -1.550196850393700920 ) ) ;
#13511 = DIRECTION ( 'NONE',  ( 0.000000000000000000, 0.000000000000000000, 1.000000000000000000 ) ) ;
#13512 = EDGE_CURVE ( 'NONE', #15905, #23049, #14326, .T. ) ;
#13513 = VECTOR ( 'NONE', #24482, 39.37007874015748143 ) ;
#13514 = CIRCLE ( 'NONE', #17144, 0.8267716535433071723 ) ;
#13515 = CARTESIAN_POINT ( 'NONE',  ( 0.03532354024591720376, -0.8267716535433071723, -0.7500000000000001110 ) ) ;
#13516 = CARTESIAN_POINT ( 'NONE',  ( -0.1141709026133645999, 0.3362336590883638343, 1.953740157480315043 ) ) ;
#13517 = ADVANCED_FACE ( 'NONE', ( #16702 ), #11390, .F. ) ;
#13518 = CARTESIAN_POINT ( 'NONE',  ( -0.5610236220428271858, 1.122047244090071949, 1.311930826979132746E-15 ) ) ;
#13519 = AXIS2_PLACEMENT_3D ( 'NONE', #17804, #3238, #26426 ) ;
#13520 = CARTESIAN_POINT ( 'NONE',  ( 0.000000000000000000, 0.000000000000000000, 0.07637795275590551769 ) ) ;
#13522 = EDGE_CURVE ( 'NONE', #19493, #3406, #11854, .T. ) ;
#13521 = CARTESIAN_POINT ( 'NONE',  ( -0.3990005999895503419, 0.4761957181735173017, 0.09684874924366436433 ) ) ;
#13523 = CARTESIAN_POINT ( 'NONE',  ( -0.3986320731132244610, -0.2308081338369635804, 0.1771653543307087630 ) ) ;
#13524 = CARTESIAN_POINT ( 'NONE',  ( 0.000000000000000000, 0.000000000000000000, -0.02362204724409448786 ) ) ;
#13525 = CARTESIAN_POINT ( 'NONE',  ( 0.4600326175560556230, 0.2268096725222457644, 1.766732283464566899 ) ) ;
#13526 = ADVANCED_FACE ( 'NONE', ( #14888 ), #5972, .T. ) ;
#13527 = CARTESIAN_POINT ( 'NONE',  ( 0.4009292313359112958, -0.2321359940638691999, 0.1494804572070806692 ) ) ;
#13528 = VERTEX_POINT ( 'NONE', #8501 ) ;
#13529 = CARTESIAN_POINT ( 'NONE',  ( 0.5925575908939920700, -0.2268709785195988371, -0.3929520615588121824 ) ) ;
#13530 = ( NAMED_UNIT ( * ) SI_UNIT ( $, .STERADIAN. ) SOLID_ANGLE_UNIT ( ) ) ;
#13531 = CIRCLE ( 'NONE', #2693, 0.3771653543307086909 ) ;
#13532 = EDGE_LOOP ( 'NONE', ( #27664, #11414, #10546, #23478 ) ) ;
#13533 = CARTESIAN_POINT ( 'NONE',  ( 0.1520645003235147619, -0.4909313315706889669, 0.05587710509139291737 ) ) ;
#13534 = ORIENTED_EDGE ( 'NONE', *, *, #4130, .T. ) ;
#13535 = AXIS2_PLACEMENT_3D ( 'NONE', #20049, #22590, #1128 ) ;
#13536 = DIRECTION ( 'NONE',  ( 0.000000000000000000, 0.000000000000000000, 1.000000000000000000 ) ) ;
#13537 = FACE_OUTER_BOUND ( 'NONE', #5434, .T. ) ;
#13538 = ORIENTED_EDGE ( 'NONE', *, *, #25590, .F. ) ;
#13539 = CARTESIAN_POINT ( 'NONE',  ( -0.07472527936312116370, 0.5671862884094760471, 0.9399606299212598381 ) ) ;
#13540 = ORIENTED_EDGE ( 'NONE', *, *, #24173, .F. ) ;
#13541 = CARTESIAN_POINT ( 'NONE',  ( -0.4811133747915324332, 0.000000000000000000, -0.2755905511811023723 ) ) ;
#13542 = VERTEX_POINT ( 'NONE', #15016 ) ;
#13543 = EDGE_CURVE ( 'NONE', #25416, #27836, #12872, .T. ) ;
#13544 = CIRCLE ( 'NONE', #4974, 0.1181102362204720091 ) ;
#13545 = FACE_OUTER_BOUND ( 'NONE', #1168, .T. ) ;
#13546 = LINE ( 'NONE', #2796, #21222 ) ;
#13547 = CARTESIAN_POINT ( 'NONE',  ( 0.5525004126151165096, 0.09742072959660433296, 0.2775610236220472093 ) ) ;
#13548 = DIRECTION ( 'NONE',  ( -1.000000000000000000, 0.000000000000000000, 0.000000000000000000 ) ) ;
#13549 = ORIENTED_EDGE ( 'NONE', *, *, #26870, .T. ) ;
#13550 = DIRECTION ( 'NONE',  ( 0.1736481776669301369, -0.9848077530122081313, 0.000000000000000000 ) ) ;
#13551 = ADVANCED_FACE ( 'NONE', ( #15690 ), #7340, .F. ) ;
#13552 = ADVANCED_FACE ( 'NONE', ( #4543 ), #9042, .T. ) ;
#13553 = B_SPLINE_CURVE_WITH_KNOTS ( 'NONE', 3,
 ( #9176, #8914, #11869, #12153, #1703, #14028, #18778, #12437, #25474, #6138, #4005, #5309, #12750, #26927, #12618, #6268, #18132, #7567, #12328, #21377, #16195, #10198, #4424, #19675, #13712, #27001, #19940, #7647, #7091, #11318, #13571, #26559, #24584, #18211 ),
 .UNSPECIFIED., .F., .F.,
 ( 4, 2, 2, 2, 2, 2, 2, 2, 2, 2, 2, 2, 2, 2, 2, 2, 4 ),
 ( 0.5000000000000000000, 0.5312500000000000000, 0.5624999999999998890, 0.5937499999999998890, 0.6249999999999998890, 0.6562499999999997780, 0.6874999999999997780, 0.7187499999999997780, 0.7499999999999997780, 0.7812499999999997780, 0.8124999999999997780, 0.8437499999999997780, 0.8749999999999997780, 0.9062499999999997780, 0.9374999999999997780, 0.9687500000000000000, 1.000000000000000000 ),
 .UNSPECIFIED. ) ;
#13554 = DIRECTION ( 'NONE',  ( 0.000000000000000000, 0.000000000000000000, -1.000000000000000000 ) ) ;
#13555 = CARTESIAN_POINT ( 'NONE',  ( 0.000000000000000000, 0.000000000000000000, 0.2362204724409449064 ) ) ;
#13556 = PLANE ( 'NONE',  #20918 ) ;
#13557 = CARTESIAN_POINT ( 'NONE',  ( -0.2904160862623610950, -0.1677079028045287690, 1.953740157480315043 ) ) ;
#13558 = DIRECTION ( 'NONE',  ( 1.000000000000000000, 0.000000000000000000, 0.000000000000000000 ) ) ;
#13559 = CARTESIAN_POINT ( 'NONE',  ( -0.3123213164514010431, 0.3731274149346439639, 0.1827409795182249053 ) ) ;
#13560 = CARTESIAN_POINT ( 'NONE',  ( 0.000000000000000000, 0.000000000000000000, -0.05856299212598425896 ) ) ;
#13561 = B_SPLINE_CURVE_WITH_KNOTS ( 'NONE', 3,
 ( #21836, #9098, #13478, #2736, #7131, #26610 ),
 .UNSPECIFIED., .F., .F.,
 ( 4, 2, 4 ),
 ( 8.213553798819532080E-14, 0.0007294428068852555104, 0.001458885613688375334 ),
 .UNSPECIFIED. ) ;
#13562 = CARTESIAN_POINT ( 'NONE',  ( -0.1288360683667815199, -0.3544784926413476200, 0.07637549214372835182 ) ) ;
#13563 = ORIENTED_EDGE ( 'NONE', *, *, #13942, .F. ) ;
#13564 = CARTESIAN_POINT ( 'NONE',  ( -0.4837521785369528482, -0.1097523286760773431, 0.2989974301286330571 ) ) ;
#13565 = CARTESIAN_POINT ( 'NONE',  ( -0.5187889641967551313, -0.1190953285357212593, 0.1322834645669291320 ) ) ;
#13566 = AXIS2_PLACEMENT_3D ( 'NONE', #13629, #16185, #5010 ) ;
#13567 = EDGE_LOOP ( 'NONE', ( #18956, #8570 ) ) ;
#13568 = DIRECTION ( 'NONE',  ( -1.000000000000000000, 0.000000000000000000, 0.000000000000000000 ) ) ;
#13569 = PLANE ( 'NONE',  #21123 ) ;
#13570 = ORIENTED_EDGE ( 'NONE', *, *, #26124, .T. ) ;
#13571 = CARTESIAN_POINT ( 'NONE',  ( -0.4954205147796584829, 0.1328023637707214100, -1.550196850393700476 ) ) ;
#13572 = CYLINDRICAL_SURFACE ( 'NONE', #13090, 0.5007874015748031704 ) ;
#13573 = ORIENTED_EDGE ( 'NONE', *, *, #22042, .T. ) ;
#13574 = ( LENGTH_UNIT ( ) NAMED_UNIT ( * ) SI_UNIT ( $, .METRE. ) ) ;
#13575 = CIRCLE ( 'NONE', #10419, 0.4010740433761567081 ) ;
#13576 = CARTESIAN_POINT ( 'NONE',  ( 0.000000000000000000, 0.000000000000000000, 0.1771653543307086520 ) ) ;
#13577 = CARTESIAN_POINT ( 'NONE',  ( 0.7845931698711713365, 0.3312401467028460722, -0.3038783524521976309 ) ) ;
#13578 = CIRCLE ( 'NONE', #976, 0.01968503937007872254 ) ;
#13579 = FACE_BOUND ( 'NONE', #2781, .T. ) ;
#13580 = DIRECTION ( 'NONE',  ( 0.000000000000000000, 0.000000000000000000, -1.000000000000000000 ) ) ;
#13581 = VECTOR ( 'NONE', #21346, 39.37007874015748143 ) ;
#13582 = ORIENTED_EDGE ( 'NONE', *, *, #4808, .T. ) ;
#13583 = CARTESIAN_POINT ( 'NONE',  ( 0.04380447413659061678, 0.3324885138898235892, 1.973425196850393970 ) ) ;
#13584 = CARTESIAN_POINT ( 'NONE',  ( -0.1968503937007874127, -0.07874015748031495954, 0.04546065111729338803 ) ) ;
#13585 = CARTESIAN_POINT ( 'NONE',  ( 0.06441834428465775808, -0.4889536969034878333, -1.550196850393700920 ) ) ;
#13586 = DIMENSIONAL_EXPONENTS ( 1.000000000000000000, 0.000000000000000000, 0.000000000000000000, 0.000000000000000000, 0.000000000000000000, 0.000000000000000000, 0.000000000000000000 ) ;
#13587 = CARTESIAN_POINT ( 'NONE',  ( 0.1188866373884869265, 0.4438564651657460614, -1.928289503579154740 ) ) ;
#13588 = CARTESIAN_POINT ( 'NONE',  ( 0.2762247810519147251, 0.4783323773986423166, 0.9202755905511811330 ) ) ;
#13589 = DIRECTION ( 'NONE',  ( 0.000000000000000000, -1.000000000000000000, 0.000000000000000000 ) ) ;
#13590 = FACE_OUTER_BOUND ( 'NONE', #9643, .T. ) ;
#13591 = CARTESIAN_POINT ( 'NONE',  ( -0.5754648248646618836, 0.4579130143403264963, 0.2763636194352788178 ) ) ;
#13592 = CARTESIAN_POINT ( 'NONE',  ( 0.3030032861725032167, 0.3454440660767328364, -1.928289503579165620 ) ) ;
#13593 = CARTESIAN_POINT ( 'NONE',  ( -0.4921259842519685179, 0.03220957031763950484, -1.569881889763779625 ) ) ;
#13594 = CIRCLE ( 'NONE', #26657, 0.4330708661417322913 ) ;
#13595 = CARTESIAN_POINT ( 'NONE',  ( -0.6165893942483189338, -0.09003804048641948776, -0.2411755456731409508 ) ) ;
#13596 = DIRECTION ( 'NONE',  ( 1.000000000000000000, 0.000000000000000000, 0.000000000000000000 ) ) ;
#13597 = CARTESIAN_POINT ( 'NONE',  ( 0.2938622683360631593, 0.000000000000000000, -3.745078740157480546 ) ) ;
#13598 = EDGE_CURVE ( 'NONE', #15443, #8047, #8906, .T. ) ;
#13599 = CARTESIAN_POINT ( 'NONE',  ( 0.4078284417476525925, 0.4849914877851788098, 0.1061598535658143105 ) ) ;
#13600 = EDGE_CURVE ( 'NONE', #12849, #12934, #22685, .T. ) ;
#13601 = AXIS2_PLACEMENT_3D ( 'NONE', #4166, #19272, #15058 ) ;
#13602 = B_SPLINE_CURVE_WITH_KNOTS ( 'NONE', 3,
 ( #11477, #613, #9481, #11613, #2708, #14951 ),
 .UNSPECIFIED., .F., .F.,
 ( 4, 2, 4 ),
 ( 0.6902184472752680433, 0.6915327610580710438, 0.6928470748408750435 ),
 .UNSPECIFIED. ) ;
#13603 = CARTESIAN_POINT ( 'NONE',  ( 0.000000000000000000, 0.000000000000000000, -0.2342519685039370358 ) ) ;
#13604 = PRODUCT_RELATED_PRODUCT_CATEGORY ( 'part', '', ( #19280 ) ) ;
#13605 = LINE ( 'NONE', #18384, #5240 ) ;
#13606 = CARTESIAN_POINT ( 'NONE',  ( 0.3988311005572732215, 0.4763376377695315300, 0.2574803149606298969 ) ) ;
#13607 = EDGE_CURVE ( 'NONE', #22651, #5888, #5574, .T. ) ;
#13608 = ORIENTED_EDGE ( 'NONE', *, *, #2477, .T. ) ;
#13609 = CARTESIAN_POINT ( 'NONE',  ( 0.02325127328499142915, 0.3543321272855671222, 1.953740157480314821 ) ) ;
#13610 = EDGE_LOOP ( 'NONE', ( #557, #26232, #25961, #13338 ) ) ;
#13611 = CARTESIAN_POINT ( 'NONE',  ( 0.2979095355690402069, -0.6203660015065080024, 0.1322834645669291320 ) ) ;
#13612 = DIRECTION ( 'NONE',  ( -1.000000000000000000, 0.000000000000000000, 0.000000000000000000 ) ) ;
#13613 = CARTESIAN_POINT ( 'NONE',  ( 0.1490609433615242285, -0.2393035190771456711, -0.4144858534716441278 ) ) ;
#13614 = ADVANCED_FACE ( 'NONE', ( #15434 ), #24957, .F. ) ;
#13615 = ORIENTED_EDGE ( 'NONE', *, *, #2293, .T. ) ;
#13616 = DIRECTION ( 'NONE',  ( 0.000000000000000000, 0.000000000000000000, 1.000000000000000000 ) ) ;
#13617 = B_SPLINE_CURVE_WITH_KNOTS ( 'NONE', 3,
 ( #24881, #9330, #887, #22765, #13725, #18509 ),
 .UNSPECIFIED., .F., .F.,
 ( 4, 2, 4 ),
 ( 0.9031406754215589583, 0.9046454396443720514, 0.9061502038671860326 ),
 .UNSPECIFIED. ) ;
#13618 = AXIS2_PLACEMENT_3D ( 'NONE', #196, #15285, #23896 ) ;
#13619 = DIRECTION ( 'NONE',  ( 0.000000000000000000, 1.000000000000000000, 0.000000000000000000 ) ) ;
#13620 = CARTESIAN_POINT ( 'NONE',  ( 0.04928467685643989765, -0.3740848232703748444, -3.100567304031760507 ) ) ;
#13621 = LINE ( 'NONE', #17973, #25618 ) ;
#13622 = CARTESIAN_POINT ( 'NONE',  ( 0.6339803004448225643, 0.1124719464477440256, 0.2359405056222393382 ) ) ;
#13623 = ORIENTED_EDGE ( 'NONE', *, *, #27118, .F. ) ;
#13624 = DIRECTION ( 'NONE',  ( 1.000000000000000000, 0.000000000000000000, 0.000000000000000000 ) ) ;
#13625 = VECTOR ( 'NONE', #2846, 39.37007874015748854 ) ;
#13626 = CARTESIAN_POINT ( 'NONE',  ( -0.6996199877990079141, 0.1008405537593297374, -0.2423665665178251771 ) ) ;
#13627 = VERTEX_POINT ( 'NONE', #19662 ) ;
#13628 = DIRECTION ( 'NONE',  ( 0.000000000000000000, 0.000000000000000000, 1.000000000000000000 ) ) ;
#13629 = CARTESIAN_POINT ( 'NONE',  ( 0.000000000000000000, 0.000000000000000000, -0.4724409448841456749 ) ) ;
#13630 = CARTESIAN_POINT ( 'NONE',  ( -0.4856708409200505283, -0.1649135259617098836, 1.747047244094488194 ) ) ;
#13631 = DIRECTION ( 'NONE',  ( -1.000000000000000000, 0.000000000000000000, 0.000000000000000000 ) ) ;
#13632 = AXIS2_PLACEMENT_3D ( 'NONE', #25046, #22368, #9925 ) ;
#13633 = EDGE_CURVE ( 'NONE', #12956, #27811, #11873, .T. ) ;
#13634 = CIRCLE ( 'NONE', #14092, 0.7283464566929134243 ) ;
#13635 = CARTESIAN_POINT ( 'NONE',  ( -0.1867299569291481776, 0.3233561589688985771, -3.115157480314960647 ) ) ;
#13636 = EDGE_CURVE ( 'NONE', #5917, #12685, #27681, .T. ) ;
#13637 = ORIENTED_EDGE ( 'NONE', *, *, #12159, .F. ) ;
#13638 = CARTESIAN_POINT ( 'NONE',  ( -0.4585215200179055817, -0.03001016326912892690, -1.928289503579156516 ) ) ;
#13639 = DIRECTION ( 'NONE',  ( -0.7071067818211409506, -0.7071067805519539728, 0.000000000000000000 ) ) ;
#13640 = EDGE_CURVE ( 'NONE', #21275, #10141, #22421, .T. ) ;
#13641 = VERTEX_POINT ( 'NONE', #6667 ) ;
#13642 = ORIENTED_EDGE ( 'NONE', *, *, #10461, .F. ) ;
#13643 = AXIS2_PLACEMENT_3D ( 'NONE', #7945, #16545, #2974 ) ;
#13644 = CARTESIAN_POINT ( 'NONE',  ( 0.5708661417322835607, 6.829619984160658046E-17, 0.9399606299212598381 ) ) ;
#13645 = ADVANCED_FACE ( 'NONE', ( #15299 ), #12787, .F. ) ;
#13646 = ORIENTED_EDGE ( 'NONE', *, *, #2466, .T. ) ;
#13647 = CARTESIAN_POINT ( 'NONE',  ( 0.1432577568504648236, 0.4218945342797248421, -1.934055118110236338 ) ) ;
#13648 = ORIENTED_EDGE ( 'NONE', *, *, #20014, .F. ) ;
#13649 = VERTEX_POINT ( 'NONE', #23905 ) ;
#13650 = DIRECTION ( 'NONE',  ( 0.000000000000000000, -0.8660254037844388186, 0.4999999999999998890 ) ) ;
#13651 = DIRECTION ( 'NONE',  ( -0.3420201433256691570, -0.9396926207859082059, 0.000000000000000000 ) ) ;
#13652 = FACE_OUTER_BOUND ( 'NONE', #8876, .T. ) ;
#13653 = CARTESIAN_POINT ( 'NONE',  ( -0.03532354024591893848, -0.8267716535433071723, 0.000000000000000000 ) ) ;
#13654 = DIRECTION ( 'NONE',  ( 0.000000000000000000, 0.000000000000000000, 1.000000000000000000 ) ) ;
#13655 = PRODUCT_DEFINITION_SHAPE ( 'NONE', 'NONE',  #27900 ) ;
#13656 = CIRCLE ( 'NONE', #3740, 0.3937007874015748254 ) ;
#13657 = CARTESIAN_POINT ( 'NONE',  ( 0.09842519685039365085, 0.2165354330708660902, -3.259753967135868180 ) ) ;
#13658 = DIRECTION ( 'NONE',  ( -1.000000000000000000, 0.000000000000000000, 4.051737956723259176E-18 ) ) ;
#13659 = CARTESIAN_POINT ( 'NONE',  ( -0.04638120790932924453, 0.3520466617657084796, 1.953740157480315043 ) ) ;
#13660 = CARTESIAN_POINT ( 'NONE',  ( -0.1771653543307086520, -0.1673228346456692994, 2.049113738730807629E-17 ) ) ;
#13661 = CIRCLE ( 'NONE', #1492, 0.01377952755905510404 ) ;
#13662 = DIRECTION ( 'NONE',  ( 0.000000000000000000, 0.000000000000000000, -1.000000000000000000 ) ) ;
#13663 = CYLINDRICAL_SURFACE ( 'NONE', #10768, 0.6299212598425196763 ) ;
#13664 = B_SPLINE_CURVE_WITH_KNOTS ( 'NONE', 3,
 ( #24454, #17822, #747, #9336, #26575, #5105 ),
 .UNSPECIFIED., .F., .F.,
 ( 4, 2, 4 ),
 ( 0.9359046326925619663, 0.9375808709372029925, 0.9392571091818430196 ),
 .UNSPECIFIED. ) ;
#13665 = DIRECTION ( 'NONE',  ( 0.000000000000000000, -1.000000000000000000, 0.000000000000000000 ) ) ;
#13666 = CARTESIAN_POINT ( 'NONE',  ( 0.3121994997598398491, -0.4069448477555819843, 1.747047244094488194 ) ) ;
#13667 = EDGE_CURVE ( 'NONE', #6287, #16503, #3940, .T. ) ;
#13668 = CARTESIAN_POINT ( 'NONE',  ( 0.2647715730835492609, -0.5498038367121063086, 0.2362204724409449064 ) ) ;
#13669 = EDGE_LOOP ( 'NONE', ( #9466, #21948, #4229, #3580, #9287, #16238 ) ) ;
#13670 = DIRECTION ( 'NONE',  ( 0.000000000000000000, 0.000000000000000000, 1.000000000000000000 ) ) ;
#13671 = CARTESIAN_POINT ( 'NONE',  ( 0.04632226222394355414, -0.3520598332081320558, 1.953740157480315043 ) ) ;
#13672 = EDGE_CURVE ( 'NONE', #18301, #18986, #193, .T. ) ;
#13673 = AXIS2_PLACEMENT_3D ( 'NONE', #11339, #22634, #19957 ) ;
#13674 = VERTEX_POINT ( 'NONE', #8771 ) ;
#13675 = DIRECTION ( 'NONE',  ( 0.000000000000000000, 0.000000000000000000, 1.000000000000000000 ) ) ;
#13676 = VERTEX_POINT ( 'NONE', #17394 ) ;
#13677 = AXIS2_PLACEMENT_3D ( 'NONE', #602, #7369, #4967 ) ;
#13678 = CARTESIAN_POINT ( 'NONE',  ( 0.2180862235769348290, -0.4423390553432507977, -1.569881889763779625 ) ) ;
#13679 = CARTESIAN_POINT ( 'NONE',  ( -0.3543307086614173596, 4.268512490100411279E-17, 1.953740157480315043 ) ) ;
#13680 = ORIENTED_EDGE ( 'NONE', *, *, #10914, .F. ) ;
#13681 = CARTESIAN_POINT ( 'NONE',  ( -0.5511811023622048555, -0.03607471876259069760, 0.9399606299212598381 ) ) ;
#13682 = ORIENTED_EDGE ( 'NONE', *, *, #1071, .T. ) ;
#13683 = EDGE_CURVE ( 'NONE', #14678, #661, #11600, .T. ) ;
#13684 = CARTESIAN_POINT ( 'NONE',  ( 0.4029514798610943083, 0.3205030004504269003, 0.3251195115615853615 ) ) ;
#13685 = AXIS2_PLACEMENT_3D ( 'NONE', #26246, #6907, #11274 ) ;
#13686 = CARTESIAN_POINT ( 'NONE',  ( 0.000000000000000000, 0.000000000000000000, 0.09685039370078740717 ) ) ;
#13687 = CARTESIAN_POINT ( 'NONE',  ( 0.1517511419331485645, 0.4888569460006513268, -0.05146517564403369632 ) ) ;
#13688 = DIRECTION ( 'NONE',  ( 0.000000000000000000, 1.000000000000000000, 0.000000000000000000 ) ) ;
#13689 = FACE_OUTER_BOUND ( 'NONE', #23396, .T. ) ;
#13690 = LINE ( 'NONE', #17905, #2060 ) ;
#13691 = PLANE ( 'NONE',  #9103 ) ;
#13692 = CARTESIAN_POINT ( 'NONE',  ( 0.4887136534576805857, -0.1122103150229257218, 0.3080453759536327385 ) ) ;
#13693 = CARTESIAN_POINT ( 'NONE',  ( -0.3175540113612211890, 0.1078280746903930443, 1.953740157480315043 ) ) ;
#13694 = CLOSED_SHELL ( 'NONE', ( #21748, #26920, #17656, #6097, #25240, #2518, #26204, #9912, #19879, #3228, #356, #16343, #2264, #16454, #9390, #14206, #27717, #10518, #4776, #17632, #19889, #6243, #150, #8076, #15587, #11224, #22065, #18707, #17323, #2912, #19752, #19977, #22810, #14325, #27198, #10751, #10042, #9248, #13293, #12673, #9511, #13980, #21856, #9133, #16924, #17450, #11073, #22973, #6040, #1752, #22586, #23906, #17333, #2942 ) ) ;
#13695 = VERTEX_POINT ( 'NONE', #7074 ) ;
#13696 = DIRECTION ( 'NONE',  ( 0.000000000000000000, 0.000000000000000000, -1.000000000000000000 ) ) ;
#13697 = DIRECTION ( 'NONE',  ( 0.000000000000000000, 0.000000000000000000, -1.000000000000000000 ) ) ;
#13698 = LINE ( 'NONE', #24855, #18886 ) ;
#13699 = CARTESIAN_POINT ( 'NONE',  ( 0.1339654526248284794, -0.4984899526255159308, 1.766732283464566899 ) ) ;
#13700 = DIRECTION ( 'NONE',  ( 0.000000000000000000, 0.9636237974020582797, 0.2672623749809110993 ) ) ;
#13701 = DIRECTION ( 'NONE',  ( 0.000000000000000000, 1.000000000000000000, 0.000000000000000000 ) ) ;
#13703 = ADVANCED_FACE ( 'NONE', ( #26148 ), #10054, .T. ) ;
#13702 = VECTOR ( 'NONE', #11445, 39.37007874015748143 ) ;
#13704 = ORIENTED_EDGE ( 'NONE', *, *, #17477, .F. ) ;
#13705 = VECTOR ( 'NONE', #24992, 39.37007874015748143 ) ;
#13706 = EDGE_CURVE ( 'NONE', #25722, #9819, #21733, .T. ) ;
#13707 = VERTEX_POINT ( 'NONE', #2543 ) ;
#13708 = CARTESIAN_POINT ( 'NONE',  ( -0.05118110236220472370, -0.6299212598425196763, 7.714310545810098438E-17 ) ) ;
#13709 = DIRECTION ( 'NONE',  ( 0.000000000000000000, 0.000000000000000000, -1.000000000000000000 ) ) ;
#13710 = CARTESIAN_POINT ( 'NONE',  ( 0.09842519685039363697, 0.2165354330708661457, -3.561114497143034630 ) ) ;
#13711 = ORIENTED_EDGE ( 'NONE', *, *, #16246, .T. ) ;
#13712 = CARTESIAN_POINT ( 'NONE',  ( -0.3381512095065914991, 0.3856568748492081866, -1.550196850393700920 ) ) ;
#13713 = AXIS2_PLACEMENT_3D ( 'NONE', #13295, #6947, #21919 ) ;
#13714 = FACE_OUTER_BOUND ( 'NONE', #21790, .T. ) ;
#13715 = VERTEX_POINT ( 'NONE', #1401 ) ;
#13716 = CARTESIAN_POINT ( 'NONE',  ( -0.2161007281678285485, -0.5956855348332250610, 0.1061598535668862309 ) ) ;
#13717 = CARTESIAN_POINT ( 'NONE',  ( 0.5309636003393858328, 1.000390209383793305, -0.2368508997780850722 ) ) ;
#13718 = ADVANCED_FACE ( 'NONE', ( #12137 ), #859, .F. ) ;
#13719 = DIRECTION ( 'NONE',  ( 0.000000000000000000, 1.000000000000000000, 0.000000000000000000 ) ) ;
#13720 = ORIENTED_EDGE ( 'NONE', *, *, #19567, .T. ) ;
#13721 = AXIS2_PLACEMENT_3D ( 'NONE', #8384, #12184, #10196 ) ;
#13722 = ORIENTED_EDGE ( 'NONE', *, *, #4465, .F. ) ;
#13723 = ORIENTED_EDGE ( 'NONE', *, *, #14242, .T. ) ;
#13724 = CARTESIAN_POINT ( 'NONE',  ( -0.02190250779246035590, 0.3346456692913385988, 1.973425196850393970 ) ) ;
#13725 = CARTESIAN_POINT ( 'NONE',  ( -0.4932478747986535628, 0.08657132889677658649, 0.2574819596263889787 ) ) ;
#13726 = CARTESIAN_POINT ( 'NONE',  ( -0.4270824798167792147, -0.2466292688015026546, -1.550196850393700920 ) ) ;
#13727 = CARTESIAN_POINT ( 'NONE',  ( 0.01230314960629921330, 1.185352029804633059E-17, 0.09679133858267717494 ) ) ;
#13728 = DIRECTION ( 'NONE',  ( 0.000000000000000000, -1.000000000000000000, 0.000000000000000000 ) ) ;
#13729 = CARTESIAN_POINT ( 'NONE',  ( -0.4783323773986625782, 0.2762247810518428381, 0.9399606299212598381 ) ) ;
#13730 = CARTESIAN_POINT ( 'NONE',  ( -0.09842519685039373412, 0.2991866959364303802, -3.272637795275590733 ) ) ;
#13731 = DIRECTION ( 'NONE',  ( 0.000000000000000000, 1.000000000000000000, 0.000000000000000000 ) ) ;
#13732 = CARTESIAN_POINT ( 'NONE',  ( -1.466875984251968630E-17, 0.000000000000000000, 0.000000000000000000 ) ) ;
#13733 = CARTESIAN_POINT ( 'NONE',  ( -0.3454440660767217341, 0.3030032861725395210, -1.928289503579147635 ) ) ;
#13734 = CIRCLE ( 'NONE', #26829, 0.01181102362204724393 ) ;
#13735 = FACE_OUTER_BOUND ( 'NONE', #17737, .T. ) ;
#13736 = DIRECTION ( 'NONE',  ( 0.5000000000000002220, 0.8660254037844383745, 0.000000000000000000 ) ) ;
#13737 = VERTEX_POINT ( 'NONE', #11580 ) ;
#13738 = DIRECTION ( 'NONE',  ( -1.000000000000000000, 0.000000000000000000, 0.000000000000000000 ) ) ;
#13739 = DIRECTION ( 'NONE',  ( -1.000000000000000000, 0.000000000000000000, 0.000000000000000000 ) ) ;
#13740 = DIRECTION ( 'NONE',  ( -0.2036417511401759084, -0.4895227362422917006, -0.8478782506317888989 ) ) ;
#13741 = ADVANCED_FACE ( 'NONE', ( #5073 ), #24059, .F. ) ;
#13742 = AXIS2_PLACEMENT_3D ( 'NONE', #23050, #6654, #26133 ) ;
#13743 = FACE_OUTER_BOUND ( 'NONE', #3348, .T. ) ;
#13744 = ORIENTED_EDGE ( 'NONE', *, *, #13607, .T. ) ;
#13745 = CARTESIAN_POINT ( 'NONE',  ( 0.3976891862754212137, 0.9951575781684135480, -0.5144425584461574941 ) ) ;
#13746 = ORIENTED_EDGE ( 'NONE', *, *, #18095, .T. ) ;
#13747 = DIRECTION ( 'NONE',  ( 0.000000000000000000, -1.000000000000000000, 0.000000000000000000 ) ) ;
#13748 = ORIENTED_EDGE ( 'NONE', *, *, #2559, .F. ) ;
#13749 = CARTESIAN_POINT ( 'NONE',  ( 0.2268989272875726881, 0.3929158813954875540, -1.934055118110236338 ) ) ;
#13750 = DIRECTION ( 'NONE',  ( 1.000000000000000000, 0.000000000000000000, 0.000000000000000000 ) ) ;
#13751 = CARTESIAN_POINT ( 'NONE',  ( 0.5731455175600789209, -0.3301167833454101141, 0.1926811207747196886 ) ) ;
#13752 = CARTESIAN_POINT ( 'NONE',  ( 0.09842519685039365085, 0.2991866959364303802, -3.266084890085740877 ) ) ;
#13753 = ADVANCED_FACE ( 'NONE', ( #22738 ), #7345, .F. ) ;
#13754 = FACE_BOUND ( 'NONE', #2633, .T. ) ;
#13755 = FACE_OUTER_BOUND ( 'NONE', #12760, .T. ) ;
#13756 = ORIENTED_EDGE ( 'NONE', *, *, #15454, .F. ) ;
#13757 = DIRECTION ( 'NONE',  ( 0.000000000000000000, 0.000000000000000000, 1.000000000000000000 ) ) ;
#13758 = CIRCLE ( 'NONE', #5179, 0.3937007874015748254 ) ;
#13759 = DIRECTION ( 'NONE',  ( 1.000000000000000000, 7.017815000000000124E-18, 0.000000000000000000 ) ) ;
#13760 = CARTESIAN_POINT ( 'NONE',  ( 0.1120675189988346587, -0.4694218845611126678, -0.3846748511993476338 ) ) ;
#13761 = CARTESIAN_POINT ( 'NONE',  ( 0.000000000000000000, 0.000000000000000000, 0.3425196850393700809 ) ) ;
#13762 = CARTESIAN_POINT ( 'NONE',  ( 0.3765118517642104257, 0.02464264302293800099, -3.100567304031763172 ) ) ;
#13763 = FACE_OUTER_BOUND ( 'NONE', #17270, .T. ) ;
#13764 = EDGE_LOOP ( 'NONE', ( #24113, #10027 ) ) ;
#13765 = EDGE_CURVE ( 'NONE', #13442, #5702, #10973, .T. ) ;
#13766 = CARTESIAN_POINT ( 'NONE',  ( -0.1970259548082058665, 0.3996230174612936392, -1.934055118110236338 ) ) ;
#13767 = TOROIDAL_SURFACE ( 'NONE', #3851, 0.6102362204724409711, 0.1299212598425196763 ) ;
#13768 = VECTOR ( 'NONE', #23092, 39.37007874015748143 ) ;
#13769 = CARTESIAN_POINT ( 'NONE',  ( -0.1970259548082058665, 0.3996230174612936392, -1.934055118110236338 ) ) ;
#13770 = B_SPLINE_CURVE_WITH_KNOTS ( 'NONE', 3,
 ( #14766, #16860, #15030, #25608, #12745, #13025, #21234, #2283, #23371, #10909, #8648, #8782, #2010, #10621, #4000, #17271, #12614, #27877, #10481, #19102, #25890, #4137, #27739, #23643, #6262, #19530, #15315, #215, #14899, #23509, #19247, #4278, #8511, #6536 ),
 .UNSPECIFIED., .F., .F.,
 ( 4, 2, 2, 2, 2, 2, 2, 2, 2, 2, 2, 2, 2, 2, 2, 2, 4 ),
 ( 0.000000000000000000, 0.03125000000000002776, 0.06250000000000005551, 0.09375000000000008327, 0.1250000000000001110, 0.1562500000000001388, 0.1875000000000001388, 0.2187500000000001388, 0.2500000000000001110, 0.2812500000000001110, 0.3125000000000001665, 0.3437500000000001665, 0.3750000000000001665, 0.4062500000000001110, 0.4375000000000001110, 0.4687500000000000555, 0.5000000000000000000 ),
 .UNSPECIFIED. ) ;
#13771 = APPLICATION_PROTOCOL_DEFINITION ( 'draft international standard', 'automotive_design', 1998, #9056 ) ;
#13772 = VERTEX_POINT ( 'NONE', #5371 ) ;
#13773 = ADVANCED_FACE ( 'NONE', ( #18195 ), #18044, .T. ) ;
#13774 = CARTESIAN_POINT ( 'NONE',  ( 0.09842519685039370636, 0.2165354330708661457, -3.272637795275590733 ) ) ;
#13775 = DIRECTION ( 'NONE',  ( 0.000000000000000000, 1.000000000000000000, 0.000000000000000000 ) ) ;
#13776 = CARTESIAN_POINT ( 'NONE',  ( 0.2268096725222443211, -0.4600326175560562336, 1.766732283464566899 ) ) ;
#13777 = CONICAL_SURFACE ( 'NONE', #18735, 0.7122990885670630323, 0.2923426493749994304 ) ;
#13778 = CARTESIAN_POINT ( 'NONE',  ( -0.5905511811023621549, 7.232166136696967594E-17, 0.9399606299212598381 ) ) ;
#13779 = EDGE_LOOP ( 'NONE', ( #3443, #26971, #5013, #4355 ) ) ;
#13780 = CARTESIAN_POINT ( 'NONE',  ( 0.04877294052296175797, -0.3702005978258584573, -3.115157480314960647 ) ) ;
#13781 = ORIENTED_EDGE ( 'NONE', *, *, #26425, .F. ) ;
#13782 = CARTESIAN_POINT ( 'NONE',  ( 0.7874015748031496509, 0.3810512208497282005, 0.1369858506767638040 ) ) ;
#13783 = CARTESIAN_POINT ( 'NONE',  ( 0.000000000000000000, 0.4692913385826771866, 0.2755905511811023723 ) ) ;
#13784 = ORIENTED_EDGE ( 'NONE', *, *, #11760, .F. ) ;
#13785 = ORIENTED_EDGE ( 'NONE', *, *, #5181, .F. ) ;
#13786 = ORIENTED_EDGE ( 'NONE', *, *, #21396, .F. ) ;
#13787 = DIRECTION ( 'NONE',  ( 0.000000000000000000, 0.000000000000000000, 1.000000000000000000 ) ) ;
#13788 = LINE ( 'NONE', #11808, #26735 ) ;
#13789 = CIRCLE ( 'NONE', #8382, 0.3740157480314960647 ) ;
#13790 = ORIENTED_EDGE ( 'NONE', *, *, #16486, .F. ) ;
#13791 = CARTESIAN_POINT ( 'NONE',  ( 0.3858397471888842523, 0.2228126397719887297, -1.934055118110236338 ) ) ;
#13792 = ORIENTED_EDGE ( 'NONE', *, *, #15166, .F. ) ;
#13793 = EDGE_LOOP ( 'NONE', ( #16504, #37, #6988, #24058 ) ) ;
#13794 = FACE_OUTER_BOUND ( 'NONE', #9867, .T. ) ;
#13795 = LINE ( 'NONE', #806, #23516 ) ;
#13796 = AXIS2_PLACEMENT_3D ( 'NONE', #22543, #9383, #26484 ) ;
#13797 = EDGE_CURVE ( 'NONE', #24109, #18597, #26981, .T. ) ;
#13798 = DIRECTION ( 'NONE',  ( 0.000000000000000000, 1.000000000000000000, 0.000000000000000000 ) ) ;
#13799 = CARTESIAN_POINT ( 'NONE',  ( 0.07668265949372614354, 0.1968503937007874127, -3.252000825552965324 ) ) ;
#13800 = DIRECTION ( 'NONE',  ( 1.000000000000000000, 0.000000000000000000, 0.000000000000000000 ) ) ;
#13801 = EDGE_CURVE ( 'NONE', #5489, #24837, #6932, .T. ) ;
#13802 = B_SPLINE_CURVE_WITH_KNOTS ( 'NONE', 3,
 ( #4460, #17713, #21697, #258, #11364, #23319, #123, #11092, #25932, #21833, #502, #17314, #26335, #3943, #4858, #381, #13473, #19579, #26067, #12926, #19714, #19980, #636, #15360, #23953, #2326, #5134, #17845, #24624, #16026, #7404, #11781, #778, #1335 ),
 .UNSPECIFIED., .F., .F.,
 ( 4, 2, 2, 2, 2, 2, 2, 2, 2, 2, 2, 2, 2, 2, 2, 2, 4 ),
 ( 0.5000000000000000000, 0.5312500000000000000, 0.5625000000000000000, 0.5937500000000000000, 0.6250000000000001110, 0.6562500000000001110, 0.6875000000000000000, 0.7187500000000001110, 0.7500000000000001110, 0.7812500000000001110, 0.8125000000000002220, 0.8437500000000002220, 0.8750000000000002220, 0.9062500000000002220, 0.9375000000000001110, 0.9687500000000001110, 1.000000000000000000 ),
 .UNSPECIFIED. ) ;
#13803 = CARTESIAN_POINT ( 'NONE',  ( -0.0006345105826668660581, 0.4803145415259079121, 0.2362204724409446843 ) ) ;
#13804 = EDGE_CURVE ( 'NONE', #26100, #26154, #9881, .T. ) ;
#13805 = CARTESIAN_POINT ( 'NONE',  ( -0.2362204724225640262, 2.892866454453686688E-17, -4.330708661417323135 ) ) ;
#13806 = PRESENTATION_STYLE_ASSIGNMENT (( #16070 ) ) ;
#13807 = CARTESIAN_POINT ( 'NONE',  ( -0.2669480828848092013, 0.2341512108694271399, 1.953740157480315043 ) ) ;
#13808 = ADVANCED_FACE ( 'NONE', ( #16109 ), #9741, .F. ) ;
#13809 = CARTESIAN_POINT ( 'NONE',  ( -0.7168072604723305652, -0.1644124225520415539, 0.1960773254398737175 ) ) ;
#13810 = CARTESIAN_POINT ( 'NONE',  ( 0.1490609433494345659, 0.2311078172902765182, -0.4192176441073949267 ) ) ;
#13811 = CARTESIAN_POINT ( 'NONE',  ( -0.3996755081322992398, 0.4756294029998582307, 0.09684874924366436433 ) ) ;
#13812 = EDGE_CURVE ( 'NONE', #9956, #24011, #10522, .T. ) ;
#13813 = AXIS2_PLACEMENT_3D ( 'NONE', #10740, #14736, #17099 ) ;
#13814 = CARTESIAN_POINT ( 'NONE',  ( 0.6397637795275591399, 0.000000000000000000, 0.000000000000000000 ) ) ;
#13815 = CARTESIAN_POINT ( 'NONE',  ( 0.4069448477556118493, -0.3121994997598555033, 1.747047244094488194 ) ) ;
#13816 = CARTESIAN_POINT ( 'NONE',  ( 0.1327036767659630079, 0.4954415918530855056, 1.766732283464566899 ) ) ;
#13817 = ORIENTED_EDGE ( 'NONE', *, *, #8901, .T. ) ;
#13818 = AXIS2_PLACEMENT_3D ( 'NONE', #2717, #22647, #20103 ) ;
#13819 = CARTESIAN_POINT ( 'NONE',  ( -0.1968503937007874127, 0.07874015748031495954, -0.04546065111729338803 ) ) ;
#13820 = ORIENTED_EDGE ( 'NONE', *, *, #13419, .T. ) ;
#13821 = DIRECTION ( 'NONE',  ( 1.000000000000000000, 0.000000000000000000, 0.000000000000000000 ) ) ;
#13822 = ORIENTED_EDGE ( 'NONE', *, *, #22256, .F. ) ;
#13823 = ORIENTED_EDGE ( 'NONE', *, *, #14612, .T. ) ;
#13824 = DIRECTION ( 'NONE',  ( 0.000000000000000000, 1.000000000000000000, 0.000000000000000000 ) ) ;
#13825 = VERTEX_POINT ( 'NONE', #7204 ) ;
#13826 = CARTESIAN_POINT ( 'NONE',  ( 0.4763861460130340286, 0.1275996891957706103, -1.569881889763779625 ) ) ;
#13827 = VERTEX_POINT ( 'NONE', #22458 ) ;
#13828 = CARTESIAN_POINT ( 'NONE',  ( -0.4300830224589641260, 0.3772436174784328244, 0.9399606299212598381 ) ) ;
#13829 = ORIENTED_EDGE ( 'NONE', *, *, #27822, .F. ) ;
#13830 = PLANE ( 'NONE',  #1789 ) ;
#13831 = CARTESIAN_POINT ( 'NONE',  ( 0.09842519685039355370, 0.5905905511811023745, -3.548228346456693050 ) ) ;
#13832 = PRODUCT_DEFINITION_FORMATION_WITH_SPECIFIED_SOURCE ( 'ANY', '', #21073, .NOT_KNOWN. ) ;
#13833 = VECTOR ( 'NONE', #21170, 39.37007874015748143 ) ;
#13834 = CARTESIAN_POINT ( 'NONE',  ( 0.4931450244001936989, 0.08715529520342342462, 0.2574827755769819038 ) ) ;
#13835 = DIRECTION ( 'NONE',  ( -1.000000000000000000, 0.000000000000000000, 0.000000000000000000 ) ) ;
#13836 = DIRECTION ( 'NONE',  ( 0.000000000000000000, 0.000000000000000000, 1.000000000000000000 ) ) ;
#13837 = DIRECTION ( 'NONE',  ( 0.000000000000000000, -1.000000000000000000, 0.000000000000000000 ) ) ;
#13838 = EDGE_CURVE ( 'NONE', #7492, #2655, #26310, .T. ) ;
#13839 = AXIS2_PLACEMENT_3D ( 'NONE', #26942, #16349, #20722 ) ;
#13840 = CARTESIAN_POINT ( 'NONE',  ( 0.5187889641967551313, -0.1190953285357214675, 0.3401574803149606252 ) ) ;
#13841 = CARTESIAN_POINT ( 'NONE',  ( 0.3175540113612412840, -0.1078280746903980958, 1.953740157480315043 ) ) ;
#13842 = EDGE_CURVE ( 'NONE', #22807, #21046, #21368, .T. ) ;
#13843 = UNCERTAINTY_MEASURE_WITH_UNIT (LENGTH_MEASURE( 1.000000000000000082E-05 ), #21076, 'distance_accuracy_value', 'NONE') ;
#13844 = ORIENTED_EDGE ( 'NONE', *, *, #24176, .T. ) ;
#13845 = CARTESIAN_POINT ( 'NONE',  ( 0.000000000000000000, 0.000000000000000000, -6.010066929133858501E-17 ) ) ;
#13846 = FACE_OUTER_BOUND ( 'NONE', #10876, .T. ) ;
#13847 = DIRECTION ( 'NONE',  ( 0.000000000000000000, 0.000000000000000000, 1.000000000000000000 ) ) ;
#13848 = CARTESIAN_POINT ( 'NONE',  ( 0.1518453844022533417, 0.2938239883722331136, 0.3972446186644590371 ) ) ;
#13849 = DIRECTION ( 'NONE',  ( -0.000000000000000000, 1.000000000000000000, -0.000000000000000000 ) ) ;
#13850 = CARTESIAN_POINT ( 'NONE',  ( -0.3100894960429780856, -0.1796141127295652340, 0.09506557084190404849 ) ) ;
#13851 = ORIENTED_EDGE ( 'NONE', *, *, #12083, .F. ) ;
#13852 = CIRCLE ( 'NONE', #20156, 0.4692913385826771866 ) ;
#13853 = EDGE_CURVE ( 'NONE', #11811, #24109, #13661, .T. ) ;
#13854 = ORIENTED_EDGE ( 'NONE', *, *, #23037, .T. ) ;
#13855 = AXIS2_PLACEMENT_3D ( 'NONE', #8267, #6167, #14793 ) ;
#13856 = DIRECTION ( 'NONE',  ( 0.000000000000000000, 1.000000000000000000, 0.000000000000000000 ) ) ;
#13857 = CARTESIAN_POINT ( 'NONE',  ( 0.000000000000000000, -0.09092130223458683158, -0.4724409448818898127 ) ) ;
#13858 = VERTEX_POINT ( 'NONE', #3223 ) ;
#13859 = CYLINDRICAL_SURFACE ( 'NONE', #25274, 0.4807043897637795493 ) ;
#13860 = ORIENTED_EDGE ( 'NONE', *, *, #10075, .F. ) ;
#13861 = CARTESIAN_POINT ( 'NONE',  ( 0.7874015748031325534, 0.2485711856858030810, -0.2766034250564945451 ) ) ;
#13862 = EDGE_CURVE ( 'NONE', #19453, #24685, #20897, .T. ) ;
#13863 = B_SPLINE_CURVE_WITH_KNOTS ( 'NONE', 3,
 ( #25973, #13108, #24523, #24124, #24253, #9541, #17748, #20293, #9129, #11266 ),
 .UNSPECIFIED., .F., .F.,
 ( 4, 2, 2, 2, 4 ),
 ( 0.000000000000000000, 0.2499999999999998890, 0.4999999999999997780, 0.7499999999999996669, 1.000000000000000000 ),
 .UNSPECIFIED. ) ;
#13864 = CARTESIAN_POINT ( 'NONE',  ( 0.06200787401574805319, 7.593774443531818500E-18, -4.015748031496062964 ) ) ;
#13865 = VERTEX_POINT ( 'NONE', #16252 ) ;
#13866 = SPHERICAL_SURFACE ( 'NONE', #19820, 0.07677362204724409722 ) ;
#13867 = ORIENTED_EDGE ( 'NONE', *, *, #20703, .T. ) ;
#13868 = ORIENTED_EDGE ( 'NONE', *, *, #12749, .F. ) ;
#13869 = VECTOR ( 'NONE', #22106, 39.37007874015748143 ) ;
#13870 = CARTESIAN_POINT ( 'NONE',  ( -0.1482986320106437217, -0.3007905576423873795, 1.973425196850393970 ) ) ;
#13871 = CARTESIAN_POINT ( 'NONE',  ( -0.1275996891957763835, -0.4763861460130486281, -1.550196850393700920 ) ) ;
#13872 = EDGE_CURVE ( 'NONE', #25766, #13094, #26749, .T. ) ;
#13873 = CARTESIAN_POINT ( 'NONE',  ( -0.5018154743073831581, -0.1152098006147909692, 0.3251195115537083846 ) ) ;
#13874 = VECTOR ( 'NONE', #13331, 39.37007874015748854 ) ;
#13875 = CARTESIAN_POINT ( 'NONE',  ( 0.5476281405333178753, -0.07214854559198131956, 0.9202755905511811330 ) ) ;
#13876 = CARTESIAN_POINT ( 'NONE',  ( 0.003937007874015826907, -4.393043307086613241E-18, 0.000000000000000000 ) ) ;
#13877 = CARTESIAN_POINT ( 'NONE',  ( 0.1180276236025431108, -0.3257325899126714552, 0.1377952755905513527 ) ) ;
#13878 = CARTESIAN_POINT ( 'NONE',  ( 0.3020979083622633565, 0.3591256245826334181, 0.07637795275590551769 ) ) ;
#13879 = CARTESIAN_POINT ( 'NONE',  ( -0.6299212598425196763, 0.9448818897637796255, 0.1771653543307086520 ) ) ;
#13880 = CARTESIAN_POINT ( 'NONE',  ( 0.1896185148830505929, -0.3289909311256231650, -3.100567304031763172 ) ) ;
#13881 = CARTESIAN_POINT ( 'NONE',  ( 0.1318897637674583401, 1.615183770381184452E-17, -4.330708661396418080 ) ) ;
#13882 = CARTESIAN_POINT ( 'NONE',  ( 0.2981382804007346454, -0.6202561546315846774, 0.3401591245381555551 ) ) ;
#13883 = DIRECTION ( 'NONE',  ( 0.000000000000000000, 0.000000000000000000, -1.000000000000000000 ) ) ;
#13884 = CARTESIAN_POINT ( 'NONE',  ( 0.3214446924536846772, 0.3840069416942866742, 0.2574803149606298969 ) ) ;
#13885 = AXIS2_PLACEMENT_3D ( 'NONE', #3216, #4933, #7066 ) ;
#13886 = EDGE_LOOP ( 'NONE', ( #26659, #15035, #10177, #14665 ) ) ;
#13887 = CYLINDRICAL_SURFACE ( 'NONE', #324, 0.5511811023622047445 ) ;
#13888 = ( GEOMETRIC_REPRESENTATION_CONTEXT ( 3 ) GLOBAL_UNCERTAINTY_ASSIGNED_CONTEXT ( ( #7344 ) ) GLOBAL_UNIT_ASSIGNED_CONTEXT ( ( #9669, #1098, #10889 ) ) REPRESENTATION_CONTEXT ( 'NONE', 'WORKASPACE' ) ) ;
#13889 = PRODUCT_DEFINITION_SHAPE ( 'NONE', 'NONE',  #27883 ) ;
#13890 = LINE ( 'NONE', #5709, #27653 ) ;
#13891 = VERTEX_POINT ( 'NONE', #8336 ) ;
#13892 = CARTESIAN_POINT ( 'NONE',  ( -0.3362554559023691048, 0.1141145734058716110, 1.953740157480314599 ) ) ;
#13893 = EDGE_LOOP ( 'NONE', ( #11313, #17170 ) ) ;
#13894 = EDGE_LOOP ( 'NONE', ( #24870, #17380 ) ) ;
#13895 = CARTESIAN_POINT ( 'NONE',  ( 0.3599896729929407679, 0.2761764805255620403, -1.934055118110236338 ) ) ;
#13896 = CARTESIAN_POINT ( 'NONE',  ( 0.4308867145614553307, -0.2480839813576496411, 0.1140743250904989875 ) ) ;
#13897 = LINE ( 'NONE', #18096, #8872 ) ;
#13898 = CARTESIAN_POINT ( 'NONE',  ( -0.03189542488298714729, 0.3133998791825584607, -3.179296722889725757 ) ) ;
#13899 = AXIS2_PLACEMENT_3D ( 'NONE', #6941, #10754, #26009 ) ;
#13900 = VECTOR ( 'NONE', #1152, 39.37007874015748854 ) ;
#13901 = DIRECTION ( 'NONE',  ( 0.000000000000000000, -1.000000000000000000, 0.000000000000000000 ) ) ;
#13902 = DIRECTION ( 'NONE',  ( -1.000000000000000000, 0.000000000000000000, 0.000000000000000000 ) ) ;
#13903 = ORIENTED_EDGE ( 'NONE', *, *, #9857, .F. ) ;
#13904 = FACE_OUTER_BOUND ( 'NONE', #26303, .T. ) ;
#13905 = LINE ( 'NONE', #27048, #21017 ) ;
#13906 = FACE_BOUND ( 'NONE', #25968, .T. ) ;
#13907 = VERTEX_POINT ( 'NONE', #23464 ) ;
#13908 = CARTESIAN_POINT ( 'NONE',  ( -0.1213180142433868958, -0.3572819248074448062, -3.100567304031760951 ) ) ;
#13909 = DIRECTION ( 'NONE',  ( 1.000000000000000000, 0.000000000000000000, 0.000000000000000000 ) ) ;
#13910 = LINE ( 'NONE', #3156, #10790 ) ;
#13911 = EDGE_CURVE ( 'NONE', #27805, #10159, #18157, .T. ) ;
#13912 = ORIENTED_EDGE ( 'NONE', *, *, #1001, .F. ) ;
#13913 = CARTESIAN_POINT ( 'NONE',  ( -0.4069519308876554664, 0.2006393256663590030, -1.934055118110236338 ) ) ;
#13914 = EDGE_CURVE ( 'NONE', #17036, #18321, #21805, .T. ) ;
#13915 = VECTOR ( 'NONE', #2706, 39.37007874015748143 ) ;
#13916 = AXIS2_PLACEMENT_3D ( 'NONE', #7836, #6687, #2433 ) ;
#13917 = APPLICATION_PROTOCOL_DEFINITION ( 'draft international standard', 'automotive_design', 1998, #8535 ) ;
#13918 = CARTESIAN_POINT ( 'NONE',  ( -0.6562077975700374433, -1.365924015748031427E-17, -0.2362204724409449064 ) ) ;
#13919 = ORIENTED_EDGE ( 'NONE', *, *, #4412, .F. ) ;
#13920 = CARTESIAN_POINT ( 'NONE',  ( -0.3681444341728476455, -0.8171366637306790581, -0.5188711171093385310 ) ) ;
#13921 = DIRECTION ( 'NONE',  ( 0.000000000000000000, 0.000000000000000000, -1.000000000000000000 ) ) ;
#13922 = CARTESIAN_POINT ( 'NONE',  ( 0.4069448477555986377, -0.3121994997598466770, 1.766732283464566899 ) ) ;
#13923 = ORIENTED_EDGE ( 'NONE', *, *, #1427, .T. ) ;
#13924 = CARTESIAN_POINT ( 'NONE',  ( 0.3267488823401750175, 0.1886891683788910201, -3.100567304031762284 ) ) ;
#13925 = CARTESIAN_POINT ( 'NONE',  ( 0.7874015748031497619, 0.3689420268555997362, 0.09918206336684766422 ) ) ;
#13926 = CARTESIAN_POINT ( 'NONE',  ( -0.5377323685532543474, 0.4294741335735779986, 0.1322818203437346463 ) ) ;
#13928 = VERTEX_POINT ( 'NONE', #3808 ) ;
#13927 = EDGE_CURVE ( 'NONE', #26909, #19035, #13222, .T. ) ;
#13929 = VERTEX_POINT ( 'NONE', #10151 ) ;
#13930 = CARTESIAN_POINT ( 'NONE',  ( -0.3430084144618599784, -0.7594774848350865915, -0.7521500857743448343 ) ) ;
#13931 = CIRCLE ( 'NONE', #3080, 0.6995255587571318490 ) ;
#13932 = CARTESIAN_POINT ( 'NONE',  ( -0.03532354024591775193, -0.6299212598425196763, 0.000000000000000000 ) ) ;
#13933 = DIRECTION ( 'NONE',  ( 0.000000000000000000, 0.000000000000000000, 1.000000000000000000 ) ) ;
#13934 = CIRCLE ( 'NONE', #8965, 0.5531496062992126150 ) ;
#13935 = VERTEX_POINT ( 'NONE', #12839 ) ;
#13936 = CARTESIAN_POINT ( 'NONE',  ( 0.02909913904661943010, -0.4446020952038907681, -1.934055118110236338 ) ) ;
#13937 = ORIENTED_EDGE ( 'NONE', *, *, #7179, .F. ) ;
#13938 = LINE ( 'NONE', #3180, #25376 ) ;
#13939 = DIRECTION ( 'NONE',  ( 0.000000000000000000, 1.000000000000000000, 0.000000000000000000 ) ) ;
#13940 = B_SPLINE_CURVE_WITH_KNOTS ( 'NONE', 3,
 ( #1233, #20149, #9831, #16203, #16339, #26783, #7431, #805, #5463, #18000, #16060, #26639, #7295 ),
 .UNSPECIFIED., .F., .F.,
 ( 4, 1, 1, 1, 1, 1, 1, 1, 1, 1, 4 ),
 ( -0.4911627496483090272, -0.4713348141022760118, -0.4508419969318550047, -0.4405955883466449730, -0.4252259754688289539, -0.4201027711762239658, -0.4098563625910129904, -0.4047331582984080023, -0.3944867497131970269, -0.3893635454205919832, -0.3833360769390280476 ),
 .UNSPECIFIED. ) ;
#13941 = EDGE_CURVE ( 'NONE', #3772, #23967, #25135, .T. ) ;
#13942 = EDGE_CURVE ( 'NONE', #527, #6591, #12806, .T. ) ;
#13943 = DIRECTION ( 'NONE',  ( -1.000000000000000000, 0.000000000000000000, 0.000000000000000000 ) ) ;
#13944 = CARTESIAN_POINT ( 'NONE',  ( -6.750021727583836750E-17, -0.5511811023622047445, 0.1377952755905511861 ) ) ;
#13945 = CARTESIAN_POINT ( 'NONE',  ( 1.456051859513969730E-17, 0.5007874015748032814, 0.2574827755769819038 ) ) ;
#13946 = DIRECTION ( 'NONE',  ( 1.000000000000000000, 0.000000000000000000, 0.000000000000000000 ) ) ;
#13947 = DIRECTION ( 'NONE',  ( 1.000000000000000000, 0.000000000000000000, 0.000000000000000000 ) ) ;
#13948 = DIRECTION ( 'NONE',  ( 1.000000000000000000, 0.000000000000000000, 0.000000000000000000 ) ) ;
#13949 = DIRECTION ( 'NONE',  ( 0.000000000000000000, 0.000000000000000000, 1.000000000000000000 ) ) ;
#13950 = CARTESIAN_POINT ( 'NONE',  ( 0.4561454261137161126, 0.08101060747726872291, 0.1494804571740294685 ) ) ;
#13951 = B_SPLINE_CURVE_WITH_KNOTS ( 'NONE', 3,
 ( #12545, #4072, #8038, #10414, #12677, #8583, #27529, #1805, #8442, #14694, #23300, #23150, #1665, #14404, #21164, #10135, #21305, #12815 ),
 .UNSPECIFIED., .F., .F.,
 ( 4, 2, 2, 2, 2, 2, 2, 2, 4 ),
 ( 0.000000000000000000, 0.06250000000000001388, 0.1250000000000000000, 0.1875000000000000000, 0.2500000000000000000, 0.3125000000000000000, 0.3749999999999999445, 0.4375000000000000000, 0.5000000000000000000 ),
 .UNSPECIFIED. ) ;
#13952 = CARTESIAN_POINT ( 'NONE',  ( -0.1141709026133623378, -0.3362336590883613363, 1.953740157480315043 ) ) ;
#13953 = AXIS2_PLACEMENT_3D ( 'NONE', #11988, #23015, #26965 ) ;
#13954 = ORIENTED_EDGE ( 'NONE', *, *, #3428, .T. ) ;
#13955 = CARTESIAN_POINT ( 'NONE',  ( 0.5511811023268710086, 6.750021727151124356E-17, 1.747047244094488194 ) ) ;
#13956 = CARTESIAN_POINT ( 'NONE',  ( -0.4561454261040128744, 0.08101060747557438380, 0.1494804572088045402 ) ) ;
#13957 = DIRECTION ( 'NONE',  ( 0.000000000000000000, 0.000000000000000000, 1.000000000000000000 ) ) ;
#13958 = AXIS2_PLACEMENT_3D ( 'NONE', #1834, #8199, #27834 ) ;
#13959 = CYLINDRICAL_SURFACE ( 'NONE', #6723, 0.2395669291338582696 ) ;
#13960 = VECTOR ( 'NONE', #7742, 39.37007874015748143 ) ;
#13961 = CARTESIAN_POINT ( 'NONE',  ( 0.4898768902087983768, 0.000000000000000000, 0.2362204724409449064 ) ) ;
#13962 = CARTESIAN_POINT ( 'NONE',  ( -0.1378076643338909391, 0.5144970376935737999, 1.747047244094488194 ) ) ;
#13963 = EDGE_LOOP ( 'NONE', ( #10961, #23980, #6951, #945, #2451 ) ) ;
#13964 = CARTESIAN_POINT ( 'NONE',  ( -0.1771653543307086520, 0.000000000000000000, 0.000000000000000000 ) ) ;
#13965 = ORIENTED_EDGE ( 'NONE', *, *, #26870, .F. ) ;
#13966 = CARTESIAN_POINT ( 'NONE',  ( 0.6710470464557992676, -0.1526433524317950818, 0.3401591245381555551 ) ) ;
#13967 = CARTESIAN_POINT ( 'NONE',  ( -0.3535065162672771932, 0.2712027394948494652, -1.934055118110236338 ) ) ;
#13968 = EDGE_CURVE ( 'NONE', #26393, #10201, #27701, .T. ) ;
#13970 = CYLINDRICAL_SURFACE ( 'NONE', #9550, 0.5322834645669292097 ) ;
#13969 = CARTESIAN_POINT ( 'NONE',  ( -0.3075341118175178856, -0.1775236553383595373, 1.953740157480314821 ) ) ;
#13971 = ORIENTED_EDGE ( 'NONE', *, *, #20690, .F. ) ;
#13972 = DIRECTION ( 'NONE',  ( 0.000000000000000000, -1.000000000000000000, 0.000000000000000000 ) ) ;
#13973 = ORIENTED_EDGE ( 'NONE', *, *, #3098, .F. ) ;
#13974 = EDGE_CURVE ( 'NONE', #13528, #25113, #210, .T. ) ;
#13975 = EDGE_LOOP ( 'NONE', ( #9830, #18021 ) ) ;
#13976 = CARTESIAN_POINT ( 'NONE',  ( -0.3707612262532960501, 0.3252100150720461658, -1.569881889763779625 ) ) ;
#13977 = CARTESIAN_POINT ( 'NONE',  ( -0.08530183727034117147, -0.03937007874015755610, -0.06819097667594038736 ) ) ;
#13978 = ORIENTED_EDGE ( 'NONE', *, *, #709, .F. ) ;
#13979 = ORIENTED_EDGE ( 'NONE', *, *, #16234, .T. ) ;
#13980 = ADVANCED_FACE ( 'NONE', ( #12566 ), #21330, .T. ) ;
#13981 = AXIS2_PLACEMENT_3D ( 'NONE', #58, #21485, #21623 ) ;
#13982 = CIRCLE ( 'NONE', #24325, 0.3722026523000413478 ) ;
#13983 = EDGE_CURVE ( 'NONE', #2155, #19119, #1513, .T. ) ;
#13984 = EDGE_CURVE ( 'NONE', #12770, #23749, #25885, .T. ) ;
#13985 = DIRECTION ( 'NONE',  ( 0.000000000000000000, 0.000000000000000000, -1.000000000000000000 ) ) ;
#13986 = CARTESIAN_POINT ( 'NONE',  ( -0.8725268807032540153, 0.000000000000000000, 0.2362204724409449619 ) ) ;
#13987 = DIRECTION ( 'NONE',  ( 1.000000000000000000, 0.000000000000000000, 0.000000000000000000 ) ) ;
#13988 = CARTESIAN_POINT ( 'NONE',  ( -4.821444091131312140E-17, -0.3937007874015748254, 0.2362204724409449064 ) ) ;
#13989 = CARTESIAN_POINT ( 'NONE',  ( 0.2720459371704843088, 0.3242117229735830830, 0.1377952755905511861 ) ) ;
#13990 = CARTESIAN_POINT ( 'NONE',  ( -0.3346456692913385988, -0.02190250779246036283, 1.953740157480315043 ) ) ;
#13991 = DIRECTION ( 'NONE',  ( 1.000000000000000000, 0.000000000000000000, 0.000000000000000000 ) ) ;
#13992 = DIRECTION ( 'NONE',  ( 0.000000000000000000, 0.000000000000000000, 1.000000000000000000 ) ) ;
#13993 = CARTESIAN_POINT ( 'NONE',  ( 0.2126900928101220500, -0.5837180524351338606, 0.2574827755769819038 ) ) ;
#13994 = DIRECTION ( 'NONE',  ( 0.000000000000000000, 0.000000000000000000, 1.000000000000000000 ) ) ;
#13995 = CARTESIAN_POINT ( 'NONE',  ( -0.4681308612729627172, -0.1074986424507606841, 0.2362204724409447676 ) ) ;
#13996 = AXIS2_PLACEMENT_3D ( 'NONE', #27606, #10204, #18821 ) ;
#13997 = CARTESIAN_POINT ( 'NONE',  ( -0.07874015748031495954, 0.04546065111729338803, -0.4724409448818898127 ) ) ;
#13998 = CIRCLE ( 'NONE', #2695, 0.06889763779527552368 ) ;
#13999 = VERTEX_POINT ( 'NONE', #14983 ) ;
#14000 = VERTEX_POINT ( 'NONE', #8192 ) ;
#14001 = DIRECTION ( 'NONE',  ( 0.000000000000000000, -1.000000000000000000, 0.000000000000000000 ) ) ;
#14002 = VERTEX_POINT ( 'NONE', #12427 ) ;
#14003 = DIRECTION ( 'NONE',  ( 0.000000000000000000, 0.000000000000000000, -1.000000000000000000 ) ) ;
#14004 = FACE_OUTER_BOUND ( 'NONE', #10733, .T. ) ;
#14005 = CARTESIAN_POINT ( 'NONE',  ( 0.09586345222254320786, 0.1968503937007873850, -3.573990933995919939 ) ) ;
#14006 = ORIENTED_EDGE ( 'NONE', *, *, #6385, .F. ) ;
#14007 = ADVANCED_FACE ( 'NONE', ( #1827 ), #1080, .T. ) ;
#14008 = DIRECTION ( 'NONE',  ( 0.000000000000000000, 0.000000000000000000, -1.000000000000000000 ) ) ;
#14009 = VERTEX_POINT ( 'NONE', #14721 ) ;
#14010 = ORIENTED_EDGE ( 'NONE', *, *, #18061, .T. ) ;
#14011 = ( NAMED_UNIT ( * ) SI_UNIT ( $, .STERADIAN. ) SOLID_ANGLE_UNIT ( ) ) ;
#14012 = EDGE_CURVE ( 'NONE', #19141, #26151, #5938, .T. ) ;
#14013 = CARTESIAN_POINT ( 'NONE',  ( 0.7871730179869745880, 0.3544754436444846335, 0.02177413181674842796 ) ) ;
#14014 = AXIS2_PLACEMENT_3D ( 'NONE', #12234, #16758, #14372 ) ;
#14015 = CARTESIAN_POINT ( 'NONE',  ( 0.06889763779527550980, 8.437527159479786693E-18, -0.3779527559055118058 ) ) ;
#14016 = VERTEX_POINT ( 'NONE', #27551 ) ;
#14017 = CARTESIAN_POINT ( 'NONE',  ( -0.04380447413658627998, 0.3324885138898243664, 1.973425196850393970 ) ) ;
#14018 = CARTESIAN_POINT ( 'NONE',  ( -0.2564944395535840860, 0.4441657790094369895, -1.550196850393700920 ) ) ;
#14019 = EDGE_CURVE ( 'NONE', #10626, #17531, #10541, .T. ) ;
#14020 = DIRECTION ( 'NONE',  ( 0.000000000000000000, 0.000000000000000000, 1.000000000000000000 ) ) ;
#14021 = CARTESIAN_POINT ( 'NONE',  ( -0.3642352168757148623, 0.4152525734086685016, 0.9399606299212598381 ) ) ;
#14022 = DIRECTION ( 'NONE',  ( 0.000000000000000000, 0.000000000000000000, 1.000000000000000000 ) ) ;
#14023 = PLANE ( 'NONE',  #14156 ) ;
#14024 = EDGE_LOOP ( 'NONE', ( #13239, #18923, #23835, #13704 ) ) ;
#14025 = CARTESIAN_POINT ( 'NONE',  ( 0.3584231247409862542, 4.473792596139210520E-17, -0.04133858267716535029 ) ) ;
#14026 = LINE ( 'NONE', #5111, #11686 ) ;
#14027 = CARTESIAN_POINT ( 'NONE',  ( 0.2313841235333768398, -0.3010840436257779529, -3.100567304031764060 ) ) ;
#14028 = CARTESIAN_POINT ( 'NONE',  ( 0.4599980997183205633, 0.2268967137093434727, -1.550196850393700920 ) ) ;
#14029 = DIRECTION ( 'NONE',  ( 0.000000000000000000, -0.8089354696471389161, -0.5878974450929028706 ) ) ;
#14030 = LINE ( 'NONE', #24205, #8379 ) ;
#14031 = B_SPLINE_CURVE_WITH_KNOTS ( 'NONE', 3,
 ( #15997, #18512, #7374, #9475, #25023, #20651, #18226, #7663, #26864, #22768, #24884, #20790, #5690, #3539, #27016, #1304, #9911, #12036 ),
 .UNSPECIFIED., .F., .F.,
 ( 4, 2, 2, 2, 2, 2, 2, 2, 4 ),
 ( 0.000000000000000000, 0.06250000000000000000, 0.1250000000000000000, 0.1875000000000000000, 0.2500000000000000000, 0.3125000000000000000, 0.3750000000000000000, 0.4375000000000000000, 0.5000000000000000000 ),
 .UNSPECIFIED. ) ;
#14032 = CARTESIAN_POINT ( 'NONE',  ( 0.4233199042375110910, 0.5034331896104039528, 0.2081850588264056445 ) ) ;
#14033 = ORIENTED_EDGE ( 'NONE', *, *, #3309, .F. ) ;
#14034 = EDGE_CURVE ( 'NONE', #13674, #3730, #6486, .T. ) ;
#14035 = CIRCLE ( 'NONE', #23059, 0.8031496062992127261 ) ;
#14036 = DIRECTION ( 'NONE',  ( 0.000000000000000000, 1.000000000000000000, 0.000000000000000000 ) ) ;
#14037 = DIRECTION ( 'NONE',  ( 0.9396926207859082059, 0.3420201433256690460, 0.000000000000000000 ) ) ;
#14038 = DIRECTION ( 'NONE',  ( -0.000000000000000000, -1.000000000000000000, -0.000000000000000000 ) ) ;
#14039 = ADVANCED_FACE ( 'NONE', ( #3651 ), #5590, .T. ) ;
#14040 = VERTEX_POINT ( 'NONE', #21037 ) ;
#14041 = CARTESIAN_POINT ( 'NONE',  ( 0.04632170870412826574, 0.3520570504768268383, 1.953740157480315043 ) ) ;
#14042 = VERTEX_POINT ( 'NONE', #16669 ) ;
#14043 = CARTESIAN_POINT ( 'NONE',  ( 0.05926487674657893168, 0.4498374011143063678, -1.934055118110236338 ) ) ;
#14044 = CONICAL_SURFACE ( 'NONE', #14531, 0.08582677165393072516, 0.7853981625000011624 ) ;
#14045 = CARTESIAN_POINT ( 'NONE',  ( 0.5981657849660177995, 0.000000000000000000, 0.000000000000000000 ) ) ;
#14046 = SPHERICAL_SURFACE ( 'NONE', #1218, 0.07677362204724409722 ) ;
#14047 = LINE ( 'NONE', #9501, #5130 ) ;
#14048 = CARTESIAN_POINT ( 'NONE',  ( 0.3713752547280854133, 0.06583429795695137920, 0.07637630750536809898 ) ) ;
#14049 = ORIENTED_EDGE ( 'NONE', *, *, #8536, .F. ) ;
#14050 = DIRECTION ( 'NONE',  ( 1.000000000000000000, 0.000000000000000000, 0.000000000000000000 ) ) ;
#14051 = CARTESIAN_POINT ( 'NONE',  ( -0.2223167940359789541, 0.2657206863494903648, 0.1478915661187940878 ) ) ;
#14052 = CARTESIAN_POINT ( 'NONE',  ( -0.1886891683788906593, -0.3267488823401751841, -3.100567304031762284 ) ) ;
#14053 = SURFACE_STYLE_USAGE ( .BOTH. , #20820 ) ;
#14054 = EDGE_CURVE ( 'NONE', #7492, #15470, #23788, .T. ) ;
#14055 = ORIENTED_EDGE ( 'NONE', *, *, #13872, .T. ) ;
#14056 = CARTESIAN_POINT ( 'NONE',  ( -0.05819755867303792046, 0.4417361510194100505, -1.934055118110236338 ) ) ;
#14057 = STYLED_ITEM ( 'NONE', ( #21627 ), #21602 ) ;
#14058 = CARTESIAN_POINT ( 'NONE',  ( -0.7874015748031496509, 0.3058301319751310920, -0.2956682880063846164 ) ) ;
#14059 = CIRCLE ( 'NONE', #21268, 0.1003956692913385990 ) ;
#14060 = ORIENTED_EDGE ( 'NONE', *, *, #26584, .T. ) ;
#14061 = CARTESIAN_POINT ( 'NONE',  ( -1.197070535079588716, 0.07874015748031491790, -1.078960298859116707 ) ) ;
#14062 = CARTESIAN_POINT ( 'NONE',  ( 0.000000000000000000, 0.000000000000000000, 0.2574803149606298969 ) ) ;
#14063 = CARTESIAN_POINT ( 'NONE',  ( 0.4069448477556118493, -0.3121994997598555033, 1.747047244094488194 ) ) ;
#14064 = VERTEX_POINT ( 'NONE', #19473 ) ;
#14065 = EDGE_LOOP ( 'NONE', ( #6851, #23109, #9751, #22203 ) ) ;
#14066 = EDGE_CURVE ( 'NONE', #26488, #25578, #12314, .T. ) ;
#14067 = CARTESIAN_POINT ( 'NONE',  ( 0.3384212623783066642, -0.1668516812751465739, -3.100567304031770277 ) ) ;
#14068 = ORIENTED_EDGE ( 'NONE', *, *, #22966, .F. ) ;
#14069 = CARTESIAN_POINT ( 'NONE',  ( -0.6088260560327825033, 1.112071903501499648, -0.05864771439951445287 ) ) ;
#14070 = DIRECTION ( 'NONE',  ( 0.000000000000000000, 0.000000000000000000, -1.000000000000000000 ) ) ;
#14071 = EDGE_CURVE ( 'NONE', #23853, #25692, #5929, .T. ) ;
#14072 = ORIENTED_EDGE ( 'NONE', *, *, #11791, .T. ) ;
#14073 = CIRCLE ( 'NONE', #17667, 0.4986013261500205074 ) ;
#14074 = CARTESIAN_POINT ( 'NONE',  ( -0.4134148064934505262, -0.5671632014791846421, -0.4652690387879091505 ) ) ;
#14075 = ORIENTED_EDGE ( 'NONE', *, *, #11042, .F. ) ;
#14076 = ORIENTED_EDGE ( 'NONE', *, *, #14941, .T. ) ;
#14077 = ORIENTED_EDGE ( 'NONE', *, *, #17821, .T. ) ;
#14078 = CARTESIAN_POINT ( 'NONE',  ( -0.2965233727166469713, 0.3524965443697188894, 0.1639447408842210907 ) ) ;
#14079 = CARTESIAN_POINT ( 'NONE',  ( 0.000000000000000000, 0.000000000000000000, 0.01181102362204724393 ) ) ;
#14080 = B_SPLINE_CURVE_WITH_KNOTS ( 'NONE', 3,
 ( #19362, #21487, #25185, #5853, #12191, #12718 ),
 .UNSPECIFIED., .F., .F.,
 ( 4, 2, 4 ),
 ( 0.5000000000000000000, 0.7500000000000001110, 1.000000000000000000 ),
 .UNSPECIFIED. ) ;
#14081 = CARTESIAN_POINT ( 'NONE',  ( 0.000000000000000000, 0.000000000000000000, 0.1377952755905511861 ) ) ;
#14082 = CARTESIAN_POINT ( 'NONE',  ( 0.000000000000000000, 0.000000000000000000, -0.2618110236220472231 ) ) ;
#14083 = DIRECTION ( 'NONE',  ( 0.000000000000000000, -1.000000000000000000, 0.000000000000000000 ) ) ;
#14084 = DIRECTION ( 'NONE',  ( -0.000000000000000000, -0.000000000000000000, -1.000000000000000000 ) ) ;
#14085 = CARTESIAN_POINT ( 'NONE',  ( 0.5188388941967637669, -0.1188778293835250077, 0.3401591244667909186 ) ) ;
#14086 = CARTESIAN_POINT ( 'NONE',  ( 0.5381367953592983699, -0.3104394140547701020, 0.2574827755769819038 ) ) ;
#14087 = AXIS2_PLACEMENT_3D ( 'NONE', #10980, #2089, #12954 ) ;
#14088 = ORIENTED_EDGE ( 'NONE', *, *, #7028, .F. ) ;
#14089 = LINE ( 'NONE', #15926, #20915 ) ;
#14090 = CARTESIAN_POINT ( 'NONE',  ( -0.5376957092749645728, -0.3112026930392425284, 0.09685039370078740717 ) ) ;
#14091 = DIRECTION ( 'NONE',  ( 1.000000000000000000, 0.000000000000000000, 0.000000000000000000 ) ) ;
#14092 = AXIS2_PLACEMENT_3D ( 'NONE', #5067, #13836, #15683 ) ;
#14093 = DIRECTION ( 'NONE',  ( -0.000000000000000000, -1.000000000000000000, -0.000000000000000000 ) ) ;
#14094 = CARTESIAN_POINT ( 'NONE',  ( -1.466875984251968630E-17, 0.000000000000000000, -0.4566929133858267376 ) ) ;
#14095 = VERTEX_POINT ( 'NONE', #17627 ) ;
#14096 = CARTESIAN_POINT ( 'NONE',  ( 0.000000000000000000, 0.07874015748031495954, 0.000000000000000000 ) ) ;
#14097 = CARTESIAN_POINT ( 'NONE',  ( 0.4777261797697469614, 0.2355331214654221850, 1.747047244094488194 ) ) ;
#14098 = FACE_OUTER_BOUND ( 'NONE', #11634, .T. ) ;
#14099 = CARTESIAN_POINT ( 'NONE',  ( 0.4069448477555425714, 0.3121994997598541155, 1.747047244094488194 ) ) ;
#14100 = ORIENTED_EDGE ( 'NONE', *, *, #8516, .T. ) ;
#14101 = DIRECTION ( 'NONE',  ( 0.9930684569549264040, -0.1175373974578370340, 0.000000000000000000 ) ) ;
#14102 = VERTEX_POINT ( 'NONE', #2648 ) ;
#14103 = CARTESIAN_POINT ( 'NONE',  ( 0.6707652279343347956, -0.1538768215240155779, 0.3401574803149606252 ) ) ;
#14104 = ( NAMED_UNIT ( * ) SI_UNIT ( $, .STERADIAN. ) SOLID_ANGLE_UNIT ( ) ) ;
#14105 = CARTESIAN_POINT ( 'NONE',  ( 0.000000000000000000, 0.5610236220472440971, -3.341531889763779686E-17 ) ) ;
#14106 = ADVANCED_FACE ( 'NONE', ( #19340 ), #630, .F. ) ;
#14107 = CARTESIAN_POINT ( 'NONE',  ( 0.3239425792934412240, 0.08676778863010829734, 1.973425196850393970 ) ) ;
#14108 = EDGE_LOOP ( 'NONE', ( #24174, #14547, #18531, #23188, #463 ) ) ;
#14109 = ORIENTED_EDGE ( 'NONE', *, *, #25627, .F. ) ;
#14110 = B_SPLINE_CURVE_WITH_KNOTS ( 'NONE', 3,
 ( #16745, #4310, #12018, #25506, #14931, #6172, #2045, #12780, #113, #12917, #10804, #6297, #8548, #17166, #19281, #25783, #21125, #14656, #25357, #10378, #21407, #17301, #10517, #4450, #21543, #20981, #6432, #14798, #2187, #15067, #18998, #23259, #1627, #3889 ),
 .UNSPECIFIED., .F., .F.,
 ( 4, 2, 2, 2, 2, 2, 2, 2, 2, 2, 2, 2, 2, 2, 2, 2, 4 ),
 ( 0.000000000000000000, 0.03125000000000001388, 0.06250000000000001388, 0.09375000000000001388, 0.1250000000000000000, 0.1562500000000000000, 0.1875000000000000278, 0.2187500000000000278, 0.2500000000000000555, 0.2812500000000000555, 0.3125000000000000555, 0.3437500000000001110, 0.3750000000000001110, 0.4062500000000000555, 0.4375000000000000000, 0.4687500000000000555, 0.5000000000000000000 ),
 .UNSPECIFIED. ) ;
#14111 = CARTESIAN_POINT ( 'NONE',  ( -0.3001918266902143251, 0.3912931228432222075, -1.569881889763779625 ) ) ;
#14112 = CARTESIAN_POINT ( 'NONE',  ( 0.4337933494688747671, -0.2502226818840338485, 0.09684793308443523374 ) ) ;
#14113 = ORIENTED_EDGE ( 'NONE', *, *, #22449, .T. ) ;
#14114 = VERTEX_POINT ( 'NONE', #25979 ) ;
#14115 = ORIENTED_EDGE ( 'NONE', *, *, #17282, .F. ) ;
#14116 = ORIENTED_EDGE ( 'NONE', *, *, #5362, .T. ) ;
#14117 = AXIS2_PLACEMENT_3D ( 'NONE', #8136, #1765, #4174 ) ;
#14118 = AXIS2_PLACEMENT_3D ( 'NONE', #16312, #12067, #24914 ) ;
#14119 = ITEM_DEFINED_TRANSFORMATION ( 'NONE', 'NONE', #7557,  #11588 ) ;
#14120 = CARTESIAN_POINT ( 'NONE',  ( 0.4932136069632150344, 0.08676634416061969335, 0.2574827755769819038 ) ) ;
#14121 = CARTESIAN_POINT ( 'NONE',  ( 0.000000000000000000, 0.000000000000000000, 0.2637795275590551491 ) ) ;
#14122 = FACE_OUTER_BOUND ( 'NONE', #12276, .T. ) ;
#14123 = DIRECTION ( 'NONE',  ( 0.000000000000000000, 0.000000000000000000, -1.000000000000000000 ) ) ;
#14124 = TOROIDAL_SURFACE ( 'NONE', #13643, 0.4232283464566928832, 0.07677165354330708902 ) ;
#14125 = VERTEX_POINT ( 'NONE', #9006 ) ;
#14126 = DIRECTION ( 'NONE',  ( 1.000000000000000000, 0.000000000000000000, 0.000000000000000000 ) ) ;
#14127 = CARTESIAN_POINT ( 'NONE',  ( -0.08676778863011463949, -0.3239425792934414461, 1.953740157480315043 ) ) ;
#14128 = EDGE_CURVE ( 'NONE', #16084, #6657, #19628, .T. ) ;
#14129 = UNCERTAINTY_MEASURE_WITH_UNIT (LENGTH_MEASURE( 1.000000000000000082E-05 ), #14822, 'distance_accuracy_value', 'NONE') ;
#14130 = ORIENTED_EDGE ( 'NONE', *, *, #20692, .F. ) ;
#14131 = DIRECTION ( 'NONE',  ( 1.000000000000000000, 0.000000000000000000, 0.000000000000000000 ) ) ;
#14132 = ADVANCED_FACE ( 'NONE', ( #17759 ), #25434, .T. ) ;
#14133 = CARTESIAN_POINT ( 'NONE',  ( 0.03008364706454716778, -0.1136516277932328595, -0.1968503937007874127 ) ) ;
#14134 = CARTESIAN_POINT ( 'NONE',  ( -0.6098077518716100709, -0.1659937022319242506, 0.2254863467269558330 ) ) ;
#14135 = DIRECTION ( 'NONE',  ( 0.000000000000000000, 0.5000000000000003331, -0.8660254037844384856 ) ) ;
#14136 = CARTESIAN_POINT ( 'NONE',  ( -0.2236164729184980104, 0.2672714825434807095, 0.1166443193980749027 ) ) ;
#14137 = PRODUCT_DEFINITION_SHAPE ( 'NONE', 'NONE',  #27904 ) ;
#14138 = DIRECTION ( 'NONE',  ( -1.000000000000000000, 0.000000000000000000, 0.000000000000000000 ) ) ;
#14139 = CONICAL_SURFACE ( 'NONE', #24049, 0.4863540308881693086, 1.365720138124999927 ) ;
#14140 = AXIS2_PLACEMENT_3D ( 'NONE', #20505, #18358, #5395 ) ;
#14141 = ORIENTED_EDGE ( 'NONE', *, *, #22256, .T. ) ;
#14142 = EDGE_CURVE ( 'NONE', #23041, #13221, #16677, .T. ) ;
#14143 = DIRECTION ( 'NONE',  ( -1.000000000000000000, 0.000000000000000000, 0.000000000000000000 ) ) ;
#14144 = ORIENTED_EDGE ( 'NONE', *, *, #10365, .F. ) ;
#14145 = EDGE_LOOP ( 'NONE', ( #16259, #8323, #18569, #7965, #14197 ) ) ;
#14146 = AXIS2_PLACEMENT_3D ( 'NONE', #4405, #19513, #202 ) ;
#14147 = DIRECTION ( 'NONE',  ( -1.000000000000000000, 0.000000000000000000, 0.000000000000000000 ) ) ;
#14148 = ( REPRESENTATION_RELATIONSHIP ('NONE','NONE', #12434, #16232 ) REPRESENTATION_RELATIONSHIP_WITH_TRANSFORMATION ( #5930 )SHAPE_REPRESENTATION_RELATIONSHIP( ) ) ;
#14149 = DIRECTION ( 'NONE',  ( 1.000000000000000000, 0.000000000000000000, 0.000000000000000000 ) ) ;
#14150 = AXIS2_PLACEMENT_3D ( 'NONE', #13289, #21772, #4401 ) ;
#14151 = CARTESIAN_POINT ( 'NONE',  ( 0.07874015748031480688, 0.1968503937007873850, -3.548228346456692162 ) ) ;
#14152 = VERTEX_POINT ( 'NONE', #24128 ) ;
#14153 = VERTEX_POINT ( 'NONE', #15258 ) ;
#14154 = SURFACE_SIDE_STYLE ('',( #9190 ) ) ;
#14155 = DIRECTION ( 'NONE',  ( 0.000000000000000000, 0.000000000000000000, -1.000000000000000000 ) ) ;
#14156 = AXIS2_PLACEMENT_3D ( 'NONE', #748, #10826, #22496 ) ;
#14157 = EDGE_CURVE ( 'NONE', #5023, #27816, #17304, .T. ) ;
#14158 = CARTESIAN_POINT ( 'NONE',  ( 0.09855118063547688156, 0.3667122560601321357, -3.100567304031763172 ) ) ;
#14159 = CARTESIAN_POINT ( 'NONE',  ( -0.1707210962531915677, -0.4707890492249701131, 0.2574803149606298969 ) ) ;
#14160 = ORIENTED_EDGE ( 'NONE', *, *, #13640, .F. ) ;
#14161 = CARTESIAN_POINT ( 'NONE',  ( 0.7873254110087903879, 0.2512946835069670426, -0.2758545172576901128 ) ) ;
#14162 = VERTEX_POINT ( 'NONE', #6635 ) ;
#14163 = CARTESIAN_POINT ( 'NONE',  ( -0.3175540113612297932, -0.1078280746904006077, 1.973425196850393970 ) ) ;
#14164 = CARTESIAN_POINT ( 'NONE',  ( -0.4441657790094409863, -0.2564944395535778687, -1.550196850393700920 ) ) ;
#14165 = CARTESIAN_POINT ( 'NONE',  ( -2.685748425196850164E-17, 0.000000000000000000, -3.115157480314960647 ) ) ;
#14166 = ADVANCED_FACE ( 'NONE', ( #4628 ), #5102, .F. ) ;
#14167 = AXIS2_PLACEMENT_3D ( 'NONE', #25278, #19051, #18623 ) ;
#14168 = SPHERICAL_SURFACE ( 'NONE', #3327, 0.07677362204724409722 ) ;
#14169 = CARTESIAN_POINT ( 'NONE',  ( 0.4152525734086270348, -0.3642352168757560515, 0.9202755905511811330 ) ) ;
#14170 = CARTESIAN_POINT ( 'NONE',  ( -0.3020416211881005175, -0.1738080303462935516, 0.1589462317895919130 ) ) ;
#14171 = EDGE_CURVE ( 'NONE', #23254, #23881, #23455, .T. ) ;
#14172 = CIRCLE ( 'NONE', #17757, 0.7480314960629921295 ) ;
#14173 = DIRECTION ( 'NONE',  ( 1.000000000000000000, 7.017814999999989339E-18, 0.000000000000000000 ) ) ;
#14174 = EDGE_LOOP ( 'NONE', ( #23071, #25020, #25226, #15640 ) ) ;
#14175 = DIRECTION ( 'NONE',  ( 0.000000000000000000, 0.000000000000000000, 1.000000000000000000 ) ) ;
#14176 = EDGE_CURVE ( 'NONE', #3027, #3819, #20019, .T. ) ;
#14177 = CARTESIAN_POINT ( 'NONE',  ( 0.06441834428467232976, 0.4889536969035311875, -1.569881889763779625 ) ) ;
#14178 = EDGE_CURVE ( 'NONE', #13235, #8311, #22254, .T. ) ;
#14179 = DIRECTION ( 'NONE',  ( 0.000000000000000000, 0.000000000000000000, -1.000000000000000000 ) ) ;
#14180 = DIRECTION ( 'NONE',  ( -0.000000000000000000, -1.000000000000000000, -0.000000000000000000 ) ) ;
#14181 = VECTOR ( 'NONE', #23499, 39.37007874015748854 ) ;
#14182 = ORIENTED_EDGE ( 'NONE', *, *, #2987, .F. ) ;
#14183 = CARTESIAN_POINT ( 'NONE',  ( 0.9842519685039370358, -2.874015748031495843, 0.2952755905511810774 ) ) ;
#14184 = LINE ( 'NONE', #11765, #26006 ) ;
#14185 = DIRECTION ( 'NONE',  ( 0.000000000000000000, 0.000000000000000000, 1.000000000000000000 ) ) ;
#14186 = ORIENTED_EDGE ( 'NONE', *, *, #12795, .F. ) ;
#14187 = CARTESIAN_POINT ( 'NONE',  ( 0.3520612535909328211, 0.04631512375351633237, 1.953740157480315487 ) ) ;
#14188 = ORIENTED_EDGE ( 'NONE', *, *, #9199, .T. ) ;
#14189 = AXIS2_PLACEMENT_3D ( 'NONE', #24170, #19793, #21921 ) ;
#14190 = CARTESIAN_POINT ( 'NONE',  ( 0.02963280468032102044, 0.4527559054764770385, -1.934055118110236338 ) ) ;
#14191 = CARTESIAN_POINT ( 'NONE',  ( 0.0006345105826660208141, 0.4803145415259080231, 0.2529987172466452994 ) ) ;
#14192 = CARTESIAN_POINT ( 'NONE',  ( 0.5731455175603656915, -0.3301167833455752043, 0.1616495878888389581 ) ) ;
#14193 = CARTESIAN_POINT ( 'NONE',  ( 0.06046764050538371016, 0.3092437473714230722, -3.193908385656448523 ) ) ;
#14194 = CIRCLE ( 'NONE', #19620, 0.1299232283464566984 ) ;
#14195 = CARTESIAN_POINT ( 'NONE',  ( 1.197070535079588716, 0.07874015748031495954, 1.078960298859116707 ) ) ;
#14196 = CARTESIAN_POINT ( 'NONE',  ( 0.07874015748031495954, 0.1968503937007874127, -3.548228346456692162 ) ) ;
#14197 = ORIENTED_EDGE ( 'NONE', *, *, #23397, .T. ) ;
#14198 = FACE_OUTER_BOUND ( 'NONE', #17479, .T. ) ;
#14199 = EDGE_LOOP ( 'NONE', ( #16880, #22022, #2789, #21576 ) ) ;
#14200 = DIRECTION ( 'NONE',  ( 0.000000000000000000, 0.000000000000000000, -1.000000000000000000 ) ) ;
#14201 = CARTESIAN_POINT ( 'NONE',  ( -0.0007595033562148819414, 0.6881885572739390167, 0.1322834645669291320 ) ) ;
#14202 = FACE_OUTER_BOUND ( 'NONE', #21453, .T. ) ;
#14203 = AXIS2_PLACEMENT_3D ( 'NONE', #19630, #26380, #17762 ) ;
#14204 = EDGE_LOOP ( 'NONE', ( #17137, #19257, #5915, #22836 ) ) ;
#14205 = CARTESIAN_POINT ( 'NONE',  ( -0.2228126397720058549, -0.3858397471888898589, -1.934055118110236338 ) ) ;
#14206 = ADVANCED_FACE ( 'NONE', ( #3048 ), #19999, .T. ) ;
#14207 = EDGE_CURVE ( 'NONE', #5007, #21690, #14089, .T. ) ;
#14208 = AXIS2_PLACEMENT_3D ( 'NONE', #24710, #14138, #13994 ) ;
#14209 = ORIENTED_EDGE ( 'NONE', *, *, #16694, .T. ) ;
#14210 = EDGE_LOOP ( 'NONE', ( #18685, #19394, #25592, #12408 ) ) ;
#14211 = ORIENTED_EDGE ( 'NONE', *, *, #8042, .T. ) ;
#14212 = AXIS2_PLACEMENT_3D ( 'NONE', #24223, #4861, #10820 ) ;
#14213 = CARTESIAN_POINT ( 'NONE',  ( -0.3338887748335570560, -1.114136943608293295, -0.8559701994470926278 ) ) ;
#14214 = FACE_OUTER_BOUND ( 'NONE', #22948, .T. ) ;
#14215 = CARTESIAN_POINT ( 'NONE',  ( 0.4856708409200665155, -0.1649135259616916482, 1.747047244094488194 ) ) ;
#14216 = ORIENTED_EDGE ( 'NONE', *, *, #5033, .T. ) ;
#14217 = DIRECTION ( 'NONE',  ( 0.000000000000000000, 0.000000000000000000, 1.000000000000000000 ) ) ;
#14218 = VERTEX_POINT ( 'NONE', #5616 ) ;
#14219 = CARTESIAN_POINT ( 'NONE',  ( -0.3384212623783144913, -0.1668516812751341671, -3.100567304031760951 ) ) ;
#14220 = CARTESIAN_POINT ( 'NONE',  ( 0.000000000000000000, 0.000000000000000000, -4.330708661417323135 ) ) ;
#14221 = CARTESIAN_POINT ( 'NONE',  ( -0.5382052855068000241, 0.4288813374988110216, 0.1322810039474933141 ) ) ;
#14222 = AXIS2_PLACEMENT_3D ( 'NONE', #16221, #1378, #7745 ) ;
#14223 = CARTESIAN_POINT ( 'NONE',  ( 0.3346456692913385988, 0.000000000000000000, 1.953740157480315043 ) ) ;
#14224 = VERTEX_POINT ( 'NONE', #13660 ) ;
#14225 = B_SPLINE_CURVE_WITH_KNOTS ( 'NONE', 3,
 ( #469, #351, #17005, #13164, #2164, #8930 ),
 .UNSPECIFIED., .F., .F.,
 ( 4, 1, 1, 4 ),
 ( 0.000000000000000000, 0.2857142857142859760, 0.5714285714285719520, 1.000000000000000000 ),
 .UNSPECIFIED. ) ;
#14226 = CARTESIAN_POINT ( 'NONE',  ( -0.4055118110236220486, 0.9448818897637796255, 0.1308464566929133654 ) ) ;
#14227 = DIRECTION ( 'NONE',  ( 1.000000000000000000, 0.000000000000000000, 0.000000000000000000 ) ) ;
#14228 = VERTEX_POINT ( 'NONE', #818 ) ;
#14229 = CARTESIAN_POINT ( 'NONE',  ( 0.2228126397719881469, 0.3858397471888846408, -1.934055118110236338 ) ) ;
#14230 = ORIENTED_EDGE ( 'NONE', *, *, #9868, .T. ) ;
#14231 = ORIENTED_EDGE ( 'NONE', *, *, #14355, .T. ) ;
#14232 = CARTESIAN_POINT ( 'NONE',  ( -0.1968503937007874127, 0.07874015748031495954, 0.04546065111729331171 ) ) ;
#14233 = DIRECTION ( 'NONE',  ( 0.4338837391175581759, -0.9009688679024190350, 0.000000000000000000 ) ) ;
#14234 = AXIS2_PLACEMENT_3D ( 'NONE', #7281, #12914, #21539 ) ;
#14235 = CARTESIAN_POINT ( 'NONE',  ( 0.09269288654273812045, -0.3460635936744816399, -3.115157480314960647 ) ) ;
#14236 = CIRCLE ( 'NONE', #8811, 0.2952755905264887182 ) ;
#14237 = CARTESIAN_POINT ( 'NONE',  ( -4.821283464566928349E-18, 0.000000000000000000, -0.3779527559055118058 ) ) ;
#14238 = DIRECTION ( 'NONE',  ( -1.224646799147353207E-16, 1.000000000000000000, 0.000000000000000000 ) ) ;
#14239 = DIRECTION ( 'NONE',  ( -0.000000000000000000, -0.000000000000000000, -1.000000000000000000 ) ) ;
#14240 = CARTESIAN_POINT ( 'NONE',  ( 0.000000000000000000, 0.9055118110236221041, -0.3831516066089791228 ) ) ;
#14241 = PLANE ( 'NONE',  #6506 ) ;
#14242 = EDGE_CURVE ( 'NONE', #550, #15744, #5564, .T. ) ;
#14243 = DIRECTION ( 'NONE',  ( 1.000000000000000000, 0.000000000000000000, 0.000000000000000000 ) ) ;
#14244 = CARTESIAN_POINT ( 'NONE',  ( 0.0006737210091407729463, 0.6438792636759185228, 0.1183902030411692757 ) ) ;
#14245 = ADVANCED_FACE ( 'NONE', ( #9407 ), #18011, .T. ) ;
#14246 = VECTOR ( 'NONE', #17692, 39.37007874015748143 ) ;
#14247 = ORIENTED_EDGE ( 'NONE', *, *, #24538, .F. ) ;
#14248 = CARTESIAN_POINT ( 'NONE',  ( 0.000000000000000000, 0.03937007874015747977, 0.000000000000000000 ) ) ;
#14249 = FACE_BOUND ( 'NONE', #27052, .T. ) ;
#14250 = DIRECTION ( 'NONE',  ( -1.000000000000000000, 0.000000000000000000, 0.000000000000000000 ) ) ;
#14251 = CARTESIAN_POINT ( 'NONE',  ( 0.000000000000000000, 0.000000000000000000, -0.1033464566929133965 ) ) ;
#14252 = CARTESIAN_POINT ( 'NONE',  ( -0.5043504886477523375, 0.1712563538833050680, 1.747047244094488194 ) ) ;
#14253 = DIRECTION ( 'NONE',  ( 0.000000000000000000, 0.000000000000000000, 1.000000000000000000 ) ) ;
#14254 = CARTESIAN_POINT ( 'NONE',  ( 0.4954415918530851726, -0.1327036767659643957, 1.766732283464566899 ) ) ;
#14255 = ORIENTED_EDGE ( 'NONE', *, *, #2066, .F. ) ;
#14256 = CARTESIAN_POINT ( 'NONE',  ( -0.09269288654274109029, 0.3460635936744927421, -3.115157480314960647 ) ) ;
#14257 = EDGE_LOOP ( 'NONE', ( #19261, #17336, #655, #26262, #20389, #23295 ) ) ;
#14258 = DIRECTION ( 'NONE',  ( 1.000000000000000000, 0.000000000000000000, 0.000000000000000000 ) ) ;
#14259 = CIRCLE ( 'NONE', #4323, 0.5322834645669292097 ) ;
#14260 = CARTESIAN_POINT ( 'NONE',  ( 0.2195865873852730354, -0.6052790189071695082, 0.1183902030380611092 ) ) ;
#14261 = ( CONVERSION_BASED_UNIT ( 'INCH', #26811 ) LENGTH_UNIT ( ) NAMED_UNIT ( #11066 ) ) ;
#14262 = CARTESIAN_POINT ( 'NONE',  ( 0.1490609433615242285, -0.4786070381542913421, 5.861244094488189820E-17 ) ) ;
#14263 = DIRECTION ( 'NONE',  ( 0.000000000000000000, 0.000000000000000000, 1.000000000000000000 ) ) ;
#14264 = EDGE_CURVE ( 'NONE', #13528, #17285, #20721, .T. ) ;
#14265 = VERTEX_POINT ( 'NONE', #2771 ) ;
#14266 = AXIS2_PLACEMENT_3D ( 'NONE', #16215, #20297, #19154 ) ;
#14267 = CARTESIAN_POINT ( 'NONE',  ( -0.4889536969035310210, -0.06441834428467370366, -1.569881889763779625 ) ) ;
#14268 = ORIENTED_EDGE ( 'NONE', *, *, #10320, .F. ) ;
#14269 = ORIENTED_EDGE ( 'NONE', *, *, #21194, .T. ) ;
#14270 = CIRCLE ( 'NONE', #11083, 0.4986013261500205074 ) ;
#14271 = CARTESIAN_POINT ( 'NONE',  ( 0.0004974201395668471654, 0.3464563358313494934, 0.1377952755905513249 ) ) ;
#14272 = DIRECTION ( 'NONE',  ( 0.000000000000000000, 0.000000000000000000, 1.000000000000000000 ) ) ;
#14273 = B_SPLINE_CURVE_WITH_KNOTS ( 'NONE', 3,
 ( #8055, #16807, #16667, #1398 ),
 .UNSPECIFIED., .F., .F.,
 ( 4, 4 ),
 ( 0.000000000000000000, 0.08984410253495091203 ),
 .UNSPECIFIED. ) ;
#14274 = DIRECTION ( 'NONE',  ( 1.000000000000000000, 0.000000000000000000, 0.000000000000000000 ) ) ;
#14275 = EDGE_CURVE ( 'NONE', #24515, #25393, #26650, .T. ) ;
#14276 = EDGE_LOOP ( 'NONE', ( #7328, #14211 ) ) ;
#14277 = DIRECTION ( 'NONE',  ( 1.000000000000000000, 0.000000000000000000, 0.000000000000000000 ) ) ;
#14278 = CARTESIAN_POINT ( 'NONE',  ( -0.4783464566929133688, 0.9448818897637796255, -1.639108661417322569E-17 ) ) ;
#14279 = DIRECTION ( 'NONE',  ( 0.000000000000000000, 0.000000000000000000, 1.000000000000000000 ) ) ;
#14280 = CIRCLE ( 'NONE', #18312, 0.3149606299212598381 ) ;
#14281 = EDGE_CURVE ( 'NONE', #285, #18101, #9705, .T. ) ;
#14282 = CARTESIAN_POINT ( 'NONE',  ( -0.5656894121276926368, -0.3210335855601377797, 0.1956008235395614858 ) ) ;
#14283 = CARTESIAN_POINT ( 'NONE',  ( -0.2223167940359792594, 0.2657206863494902538, 0.1377952755905513249 ) ) ;
#14284 = CARTESIAN_POINT ( 'NONE',  ( 0.000000000000000000, 0.000000000000000000, 0.000000000000000000 ) ) ;
#14285 = ORIENTED_EDGE ( 'NONE', *, *, #6699, .T. ) ;
#14286 = ORIENTED_EDGE ( 'NONE', *, *, #26922, .T. ) ;
#14287 = ORIENTED_EDGE ( 'NONE', *, *, #8725, .F. ) ;
#14288 = CIRCLE ( 'NONE', #15717, 0.6299212598425196763 ) ;
#14289 = CARTESIAN_POINT ( 'NONE',  ( -0.3222028160008074682, 0.3833711078595924970, 0.09684874903502814492 ) ) ;
#14290 = AXIS2_PLACEMENT_3D ( 'NONE', #20393, #24763, #18251 ) ;
#14291 = CARTESIAN_POINT ( 'NONE',  ( 0.3726024258163779246, 0.000000000000000000, -3.115157480314960647 ) ) ;
#14292 = ORIENTED_EDGE ( 'NONE', *, *, #1876, .T. ) ;
#14293 = CARTESIAN_POINT ( 'NONE',  ( -0.2990496115119744003, -0.6198172806990825956, 0.3401591245381551110 ) ) ;
#14294 = VERTEX_POINT ( 'NONE', #20305 ) ;
#14295 = EDGE_CURVE ( 'NONE', #16467, #7047, #12342, .T. ) ;
#14296 = AXIS2_PLACEMENT_3D ( 'NONE', #3278, #27038, #7685 ) ;
#14297 = CARTESIAN_POINT ( 'NONE',  ( -0.0005980912172654155416, 0.4999996422861965883, 0.1496602734623783681 ) ) ;
#14298 = CARTESIAN_POINT ( 'NONE',  ( -0.8725268807032540153, 0.000000000000000000, -1.052618110236220428 ) ) ;
#14299 = DIRECTION ( 'NONE',  ( 1.000000000000000000, 0.000000000000000000, 0.000000000000000000 ) ) ;
#14300 = ORIENTED_EDGE ( 'NONE', *, *, #25752, .F. ) ;
#14301 = LINE ( 'NONE', #10323, #22322 ) ;
#14302 = EDGE_CURVE ( 'NONE', #10388, #3132, #19571, .T. ) ;
#14303 = ORIENTED_EDGE ( 'NONE', *, *, #3098, .T. ) ;
#14304 = CYLINDRICAL_SURFACE ( 'NONE', #4629, 0.1771653543307086798 ) ;
#14305 = DIRECTION ( 'NONE',  ( -0.9396926207859082059, 0.3420201433256691015, 0.000000000000000000 ) ) ;
#14306 = VECTOR ( 'NONE', #26841, 39.37007874015748143 ) ;
#14307 = DIRECTION ( 'NONE',  ( 0.000000000000000000, 0.000000000000000000, 1.000000000000000000 ) ) ;
#14308 = ORIENTED_EDGE ( 'NONE', *, *, #3295, .F. ) ;
#14309 = B_SPLINE_SURFACE_WITH_KNOTS ( 'NONE', 2, 3, ( 
 ( #1311, #13593, #17825, #2843, #18233, #7379, #20521, #7237, #11480, #3400, #2981, #24458, #1037, #16149, #5408, #9778, #752, #1177, #14177, #26871, #9340, #18371, #9483, #15853, #7523, #17948, #7670, #18079, #24747, #16287, #5547, #12042, #20659, #27443, #16419, #25490, #3874, #16883, #12204, #16315, #18688, #16584, #5866, #12491, #8119, #23095, #1338, #3725, #20967, #1611, #10640, #21530, #13317, #21802, #2440, #24055, #26177, #2172, #17151, #17565, #21945, #19546, #8801, #14916, #4156, #8398 ),
 ( #25767, #25908, #17418, #21392, #23795, #26041, #2569, #19406, #15182, #11065, #99, #8665, #6417, #15049, #27755, #6557, #4439, #13044, #2297, #19263, #17016, #2028, #23664, #6694, #4295, #15334, #23930, #19690, #360, #15458, #15593, #3119, #24738, #17817, #11748, #24322, #4972, #7228, #20085, #2972, #9070, #5399, #11335, #11607, #18071, #3251, #605, #13585, #888, #477, #26435, #13871, #22069, #24595, #13445, #24195, #20367, #26715, #22206, #13726, #2834, #9474, #20228, #26862, #1025, #9620 ),
 ( #11471, #742, #22346, #7373, #15996, #7514, #19815, #5250, #16142, #9331, #17683, #14018, #17939, #26569, #22491, #6971, #22630, #15848, #2700, #26306, #19951, #4829, #24448, #5100, #14601, #1716, #10179, #21067, #1303, #25452, #27159, #25022, #22766, #8088, #23066, #22919, #8225, #6117, #9768, #18652, #3392, #5687, #18510, #5832, #18797, #27433, #3839, #23359, #16700, #14754, #1434, #11892, #23205, #7801, #9909, #14455, #27015, #25312, #16408, #14164, #20512, #12035, #24882, #5971, #3538, #12459 ) ),
 .UNSPECIFIED., .F., .T., .F.,
 ( 3, 3 ),
 ( 4, 2, 2, 2, 2, 2, 2, 2, 2, 2, 2, 2, 2, 2, 2, 2, 2, 2, 2, 2, 2, 2, 2, 2, 2, 2, 2, 2, 2, 2, 2, 2, 4 ),
 ( 0.000000000000000000, 1.000000000000000000 ),
 ( 0.000000000000000000, 0.1963495408493620697, 0.3926990816987241395, 0.5890486225480862092, 0.7853981633974482790, 0.9817477042468103487, 1.178097245096172418, 1.374446785945534488, 1.570796326794896558, 1.767145867644258628, 1.963495408493620697, 2.159844949342982545, 2.356194490192344837, 2.552544031041707129, 2.748893571891068976, 2.945243112740430824, 3.141592653589793116, 3.337942194439155408, 3.534291735288517255, 3.730641276137879103, 3.926990816987241395, 4.123340357836603687, 4.319689898685965090, 4.516039439535327382, 4.712388980384689674, 4.908738521234051966, 5.105088062083414258, 5.301437602932775661, 5.497787143782137953, 5.694136684631500245, 5.890486225480861648, 6.086835766330223940, 6.283185307179586232 ),
 .UNSPECIFIED. ) ;
#14310 = CARTESIAN_POINT ( 'NONE',  ( -0.3937007874015748254, 4.893765752498281459E-17, 0.01181102362204724393 ) ) ;
#14311 = AXIS2_PLACEMENT_3D ( 'NONE', #5833, #1436, #13009 ) ;
#14312 = PRESENTATION_LAYER_ASSIGNMENT (  '', '', ( #15229 ) ) ;
#14313 = CARTESIAN_POINT ( 'NONE',  ( 0.3976891862754212137, 0.7181140751201200434, -0.6642661073933326943 ) ) ;
#14314 = DIRECTION ( 'NONE',  ( -1.000000000000000000, 0.000000000000000000, 0.000000000000000000 ) ) ;
#14315 = ORIENTED_EDGE ( 'NONE', *, *, #5465, .F. ) ;
#14316 = ORIENTED_EDGE ( 'NONE', *, *, #3659, .F. ) ;
#14317 = DIRECTION ( 'NONE',  ( 0.9948933285935716020, 0.1009319806602630709, 0.000000000000000000 ) ) ;
#14318 = LINE ( 'NONE', #8102, #9273 ) ;
#14319 = ORIENTED_EDGE ( 'NONE', *, *, #21493, .T. ) ;
#14320 = DIRECTION ( 'NONE',  ( -1.000000000000000000, 0.000000000000000000, 0.000000000000000000 ) ) ;
#14321 = CARTESIAN_POINT ( 'NONE',  ( 0.06200787401574803931, 0.000000000000000000, 0.5905511811023621549 ) ) ;
#14322 = ORIENTED_EDGE ( 'NONE', *, *, #25909, .T. ) ;
#14323 = DIRECTION ( 'NONE',  ( 0.000000000000000000, 0.000000000000000000, 1.000000000000000000 ) ) ;
#14324 = ORIENTED_EDGE ( 'NONE', *, *, #25329, .F. ) ;
#14325 = ADVANCED_FACE ( 'NONE', ( #18302 ), #14637, .T. ) ;
#14326 = B_SPLINE_CURVE_WITH_KNOTS ( 'NONE', 3,
 ( #21221, #1862, #27864, #10469, #19086, #23207 ),
 .UNSPECIFIED., .F., .F.,
 ( 4, 2, 4 ),
 ( 0.5000000000000000000, 0.7500000000000000000, 1.000000000000000000 ),
 .UNSPECIFIED. ) ;
#14327 = CARTESIAN_POINT ( 'NONE',  ( 0.6202606299212598540, -6.779653543307085645E-20, 0.000000000000000000 ) ) ;
#14328 = CARTESIAN_POINT ( 'NONE',  ( 0.000000000000000000, 0.000000000000000000, 0.1771653543307086520 ) ) ;
#14329 = AXIS2_PLACEMENT_3D ( 'NONE', #25042, #5705, #5556 ) ;
#14330 = VECTOR ( 'NONE', #20120, 39.37007874015748143 ) ;
#14331 = DIRECTION ( 'NONE',  ( 0.000000000000000000, 0.000000000000000000, 1.000000000000000000 ) ) ;
#14332 = DIRECTION ( 'NONE',  ( 0.000000000000000000, 0.000000000000000000, 1.000000000000000000 ) ) ;
#14333 = EDGE_LOOP ( 'NONE', ( #27526, #24628, #22831 ) ) ;
#14334 = FACE_BOUND ( 'NONE', #25180, .T. ) ;
#14335 = ADVANCED_FACE ( 'NONE', ( #26505 ), #26768, .F. ) ;
#14336 = VERTEX_POINT ( 'NONE', #17880 ) ;
#14337 = CARTESIAN_POINT ( 'NONE',  ( -0.3012109481301850633, 0.3598698725862389813, 0.07637795275590551769 ) ) ;
#14338 = CARTESIAN_POINT ( 'NONE',  ( 0.7874015748031496509, -0.6060691875862775913, 0.08482860590295551728 ) ) ;
#14339 = CYLINDRICAL_SURFACE ( 'NONE', #24032, 0.2362204724225640262 ) ;
#14340 = EDGE_CURVE ( 'NONE', #11508, #23587, #7866, .T. ) ;
#14341 = ORIENTED_EDGE ( 'NONE', *, *, #3995, .T. ) ;
#14342 = CARTESIAN_POINT ( 'NONE',  ( 0.3349573549949907414, 0.2938049579018708890, -1.934055118110236338 ) ) ;
#14343 = DIRECTION ( 'NONE',  ( -0.000000000000000000, -1.000000000000000000, -0.000000000000000000 ) ) ;
#14344 = ORIENTED_EDGE ( 'NONE', *, *, #6448, .T. ) ;
#14345 = ORIENTED_EDGE ( 'NONE', *, *, #23172, .F. ) ;
#14346 = ORIENTED_EDGE ( 'NONE', *, *, #20836, .T. ) ;
#14347 = ORIENTED_EDGE ( 'NONE', *, *, #5192, .F. ) ;
#14348 = PRODUCT_DEFINITION_FORMATION_WITH_SPECIFIED_SOURCE ( 'ANY', '', #13189, .NOT_KNOWN. ) ;
#14349 = AXIS2_PLACEMENT_3D ( 'NONE', #22662, #27047, #18543 ) ;
#14350 = CARTESIAN_POINT ( 'NONE',  ( 0.07874015748031495954, 0.1968503937007873850, -3.272637795275590733 ) ) ;
#14351 = CARTESIAN_POINT ( 'NONE',  ( 0.03532354024591720376, -0.8267716535433071723, 0.000000000000000000 ) ) ;
#14352 = CARTESIAN_POINT ( 'NONE',  ( -0.2663596103035606455, 0.4612490782034870396, 1.747047244094488194 ) ) ;
#14353 = SURFACE_STYLE_FILL_AREA ( #18705 ) ;
#14354 = ORIENTED_EDGE ( 'NONE', *, *, #17265, .F. ) ;
#14355 = EDGE_CURVE ( 'NONE', #25308, #17724, #6049, .T. ) ;
#14356 = AXIS2_PLACEMENT_3D ( 'NONE', #9795, #5426, #10487 ) ;
#14357 = CARTESIAN_POINT ( 'NONE',  ( 0.3765118517642104257, 0.02464264302293800099, -3.100567304031763172 ) ) ;
#14358 = CYLINDRICAL_SURFACE ( 'NONE', #27789, 0.5511811023622047445 ) ;
#14359 = LINE ( 'NONE', #7718, #7305 ) ;
#14360 = CARTESIAN_POINT ( 'NONE',  ( -0.1775730735577547292, 0.3074993854542629190, 1.953740157480315043 ) ) ;
#14361 = ORIENTED_EDGE ( 'NONE', *, *, #298, .T. ) ;
#14362 = ORIENTED_EDGE ( 'NONE', *, *, #22572, .T. ) ;
#14363 = EDGE_CURVE ( 'NONE', #5266, #19648, #17657, .T. ) ;
#14364 = CARTESIAN_POINT ( 'NONE',  ( -0.3602580257949353215, -0.7074757604431674007, -0.6452024007641304904 ) ) ;
#14366 = CARTESIAN_POINT ( 'NONE',  ( -0.03736310157557561074, 0.5708661417322835607, 0.9399606299212598381 ) ) ;
#14365 = DIRECTION ( 'NONE',  ( -0.000000000000000000, -1.000000000000000000, -0.000000000000000000 ) ) ;
#14367 = B_SPLINE_CURVE_WITH_KNOTS ( 'NONE', 3,
 ( #12504, #12638, #16890, #17026, #27765, #25073 ),
 .UNSPECIFIED., .F., .F.,
 ( 4, 2, 4 ),
 ( 0.000000000000000000, 0.2500000000000000000, 0.5000000000000000000 ),
 .UNSPECIFIED. ) ;
#14368 = ORIENTED_EDGE ( 'NONE', *, *, #12729, .T. ) ;
#14369 = VERTEX_POINT ( 'NONE', #21294 ) ;
#14370 = ORIENTED_EDGE ( 'NONE', *, *, #24231, .T. ) ;
#14371 = DIRECTION ( 'NONE',  ( 0.9848077530122080203, -0.1736481776669309973, 0.000000000000000000 ) ) ;
#14372 = DIRECTION ( 'NONE',  ( 0.000000000000000000, 0.000000000000000000, -1.000000000000000000 ) ) ;
#14373 = EDGE_CURVE ( 'NONE', #16756, #21681, #5766, .T. ) ;
#14374 = CIRCLE ( 'NONE', #1707, 0.4807043897637795493 ) ;
#14375 = AXIS2_PLACEMENT_3D ( 'NONE', #18803, #27728, #19090 ) ;
#14376 = CARTESIAN_POINT ( 'NONE',  ( -0.3213305936751578717, -0.1584254766472200371, -3.115157480314960647 ) ) ;
#14377 = CARTESIAN_POINT ( 'NONE',  ( -0.5511811023622046335, -0.07214943758244286853, 0.9202755905511811330 ) ) ;
#14378 = VECTOR ( 'NONE', #19688, 39.37007874015748143 ) ;
#14379 = CARTESIAN_POINT ( 'NONE',  ( -0.7874015748031496509, -5.862181872598426086E-06, -1.869015748010449007 ) ) ;
#14380 = PLANE ( 'NONE',  #873 ) ;
#14381 = CARTESIAN_POINT ( 'NONE',  ( 0.000000000000000000, 0.000000000000000000, -0.2342519685039370358 ) ) ;
#14382 = DIRECTION ( 'NONE',  ( 0.000000000000000000, 0.000000000000000000, -1.000000000000000000 ) ) ;
#14383 = B_SPLINE_CURVE_WITH_KNOTS ( 'NONE', 3,
 ( #18980, #18828, #3430, #5577, #10083, #11930, #1609, #12068, #18402, #24775, #27051, #20549, #5864, #9943, #10214, #14641, #14489, #16726, #18547, #21107, #27194, #27468, #7700, #7841, #8117, #16583, #16446, #23239, #5724, #1749, #5440, #3568, #12202, #25198 ),
 .UNSPECIFIED., .F., .F.,
 ( 4, 2, 2, 2, 2, 2, 2, 2, 2, 2, 2, 2, 2, 2, 2, 2, 4 ),
 ( 0.5000000000000000000, 0.5312500000000000000, 0.5625000000000000000, 0.5937500000000000000, 0.6250000000000000000, 0.6562500000000000000, 0.6875000000000000000, 0.7187500000000000000, 0.7500000000000000000, 0.7812500000000000000, 0.8125000000000001110, 0.8437500000000000000, 0.8750000000000000000, 0.9062500000000000000, 0.9375000000000000000, 0.9687500000000000000, 1.000000000000000000 ),
 .UNSPECIFIED. ) ;
#14385 = CARTESIAN_POINT ( 'NONE',  ( 0.5385210225480960844, 0.4284847435812472183, 0.3401574803149606252 ) ) ;
#14384 = AXIS2_PLACEMENT_3D ( 'NONE', #12990, #10874, #21896 ) ;
#14386 = EDGE_CURVE ( 'NONE', #10869, #6124, #18292, .T. ) ;
#14387 = CARTESIAN_POINT ( 'NONE',  ( -0.0005855335178275720065, 0.4865383137617886322, 0.1075369453640087208 ) ) ;
#14388 = CARTESIAN_POINT ( 'NONE',  ( 0.000000000000000000, 0.4724409448818898127, -1.988188976448617584 ) ) ;
#14389 = DIRECTION ( 'NONE',  ( 1.000000000000000000, 0.000000000000000000, 0.000000000000000000 ) ) ;
#14390 = DIRECTION ( 'NONE',  ( 1.000000000000000000, 0.000000000000000000, 0.000000000000000000 ) ) ;
#14391 = FACE_OUTER_BOUND ( 'NONE', #79, .T. ) ;
#14392 = FILL_AREA_STYLE_COLOUR ( '', #23961 ) ;
#14393 = APPLICATION_PROTOCOL_DEFINITION ( 'draft international standard', 'automotive_design', 1998, #13230 ) ;
#14394 = CARTESIAN_POINT ( 'NONE',  ( 0.000000000000000000, 0.1968503937007875237, 0.000000000000000000 ) ) ;
#14395 = ADVANCED_BREP_SHAPE_REPRESENTATION ( 'Front Bearing Cover', ( #3076, #11588 ), #10253 ) ;
#14396 = CARTESIAN_POINT ( 'NONE',  ( -0.3855916753051397139, 0.3382184156732160329, 1.766732283464566899 ) ) ;
#14397 = CIRCLE ( 'NONE', #5817, 0.4330708661417322913 ) ;
#14398 = EDGE_LOOP ( 'NONE', ( #26277, #27213, #11239, #466, #14441 ) ) ;
#14399 = ORIENTED_EDGE ( 'NONE', *, *, #22840, .T. ) ;
#14400 = CIRCLE ( 'NONE', #3530, 0.3937007874015748254 ) ;
#14401 = CARTESIAN_POINT ( 'NONE',  ( -0.6751968503937006982, 0.000000000000000000, -0.2755905511811023723 ) ) ;
#14402 = ORIENTED_EDGE ( 'NONE', *, *, #25712, .F. ) ;
#14403 = CIRCLE ( 'NONE', #2199, 0.4842519685039370358 ) ;
#14404 = CARTESIAN_POINT ( 'NONE',  ( 0.3666644560843324574, -0.2817828961649161967, -1.928289503579156294 ) ) ;
#14405 = CARTESIAN_POINT ( 'NONE',  ( 0.3976891862754212137, 0.7181140751201200434, -0.6642661073933326943 ) ) ;
#14406 = DIRECTION ( 'NONE',  ( 0.000000000000000000, 0.000000000000000000, -1.000000000000000000 ) ) ;
#14407 = EDGE_LOOP ( 'NONE', ( #7756, #6132, #7402, #20506, #27533 ) ) ;
#14408 = EDGE_CURVE ( 'NONE', #13542, #10528, #3615, .T. ) ;
#14409 = CARTESIAN_POINT ( 'NONE',  ( -0.4423390553432706152, 0.2180862235769438773, -1.550196850393700920 ) ) ;
#14410 = EDGE_CURVE ( 'NONE', #21729, #22901, #20469, .T. ) ;
#14411 = VECTOR ( 'NONE', #3281, 39.37007874015748854 ) ;
#14412 = ORIENTED_EDGE ( 'NONE', *, *, #11215, .F. ) ;
#14413 = EDGE_CURVE ( 'NONE', #26100, #657, #24078, .T. ) ;
#14414 = CONTEXT_DEPENDENT_SHAPE_REPRESENTATION ( #20989, #3042 ) ;
#14415 = CARTESIAN_POINT ( 'NONE',  ( -0.09139240964747702423, 0.07874015748031500117, -1.981023540891279271E-18 ) ) ;
#14416 = CARTESIAN_POINT ( 'NONE',  ( 0.2122766679520240174, -0.5838685267775873822, 0.09684793308443542803 ) ) ;
#14417 = FACE_OUTER_BOUND ( 'NONE', #4170, .T. ) ;
#14418 = EDGE_CURVE ( 'NONE', #5922, #4895, #10097, .T. ) ;
#14419 = ORIENTED_EDGE ( 'NONE', *, *, #16954, .F. ) ;
#14420 = CARTESIAN_POINT ( 'NONE',  ( 0.000000000000000000, 0.000000000000000000, -0.2480314960629921295 ) ) ;
#14421 = DIRECTION ( 'NONE',  ( 0.000000000000000000, 1.000000000000000000, 0.000000000000000000 ) ) ;
#14422 = CIRCLE ( 'NONE', #4486, 0.3771653543307086909 ) ;
#14423 = UNCERTAINTY_MEASURE_WITH_UNIT (LENGTH_MEASURE( 1.000000000000000082E-05 ), #309, 'distance_accuracy_value', 'NONE') ;
#14424 = DIRECTION ( 'NONE',  ( 1.000000000000000000, 0.000000000000000000, 0.000000000000000000 ) ) ;
#14425 = DIRECTION ( 'NONE',  ( 0.000000000000000000, 1.000000000000000000, 0.000000000000000000 ) ) ;
#14426 = CARTESIAN_POINT ( 'NONE',  ( -0.5365253175192220558, -0.4262145198643368937, 0.1637104082999795707 ) ) ;
#14427 = MECHANICAL_DESIGN_GEOMETRIC_PRESENTATION_REPRESENTATION (  '', ( #4915 ), #5845 ) ;
#14428 = FACE_OUTER_BOUND ( 'NONE', #4746, .T. ) ;
#14429 = CARTESIAN_POINT ( 'NONE',  ( 0.5525004126151165096, 0.09742072959660433296, 0.1771653543307086520 ) ) ;
#14430 = ( BOUNDED_CURVE ( )  B_SPLINE_CURVE ( 3, ( #4814, #11591, #18055, #13427 ),
 .UNSPECIFIED., .F., .T. ) 
 B_SPLINE_CURVE_WITH_KNOTS ( ( 4, 4 ),
 ( 3.028426401679942259, 3.254758905499644417 ),
 .UNSPECIFIED. ) 
 CURVE ( )  GEOMETRIC_REPRESENTATION_ITEM ( )  RATIONAL_B_SPLINE_CURVE ( ( 1.000000000000000000, 0.9957356870045847019, 0.9957356870045847019, 1.000000000000000000 ) ) 
 REPRESENTATION_ITEM ( '' )  ) ;
#14431 = EDGE_LOOP ( 'NONE', ( #23312, #15590, #17168, #9866 ) ) ;
#14432 = EDGE_LOOP ( 'NONE', ( #12826, #8073, #13781, #7226 ) ) ;
#14433 = CARTESIAN_POINT ( 'NONE',  ( -0.1968503937007874127, -3.496765354330708585E-17, -0.09092130223458683158 ) ) ;
#14434 = ORIENTED_EDGE ( 'NONE', *, *, #19173, .F. ) ;
#14435 = ADVANCED_FACE ( 'NONE', ( #3768 ), #23673, .T. ) ;
#14436 = AXIS2_PLACEMENT_3D ( 'NONE', #11367, #2868, #23957 ) ;
#14437 = CARTESIAN_POINT ( 'NONE',  ( -9.069736220472442904E-16, -0.8267716535433071723, -0.7883858267716535861 ) ) ;
#14438 = CARTESIAN_POINT ( 'NONE',  ( -0.4426630059400472605, 0.000000000000000000, -0.2480314960629921295 ) ) ;
#14439 = DIRECTION ( 'NONE',  ( 0.000000000000000000, 0.000000000000000000, 1.000000000000000000 ) ) ;
#14440 = CARTESIAN_POINT ( 'NONE',  ( 0.000000000000000000, 0.000000000000000000, -0.2342519685039370358 ) ) ;
#14441 = ORIENTED_EDGE ( 'NONE', *, *, #19919, .F. ) ;
#14442 = FACE_OUTER_BOUND ( 'NONE', #27609, .T. ) ;
#14443 = EDGE_CURVE ( 'NONE', #15671, #7941, #20488, .T. ) ;
#14444 = CARTESIAN_POINT ( 'NONE',  ( 0.06889763779527550980, 8.437527159479786693E-18, -0.02362204724409468909 ) ) ;
#14445 = ORIENTED_EDGE ( 'NONE', *, *, #17628, .T. ) ;
#14446 = EDGE_CURVE ( 'NONE', #11422, #9678, #27790, .T. ) ;
#14447 = CARTESIAN_POINT ( 'NONE',  ( -4.821444091131312140E-17, -0.3937007874015748254, 0.02362204724409448786 ) ) ;
#14448 = DIRECTION ( 'NONE',  ( -1.000000000000000000, 0.000000000000000000, 0.000000000000000000 ) ) ;
#14449 = DIRECTION ( 'NONE',  ( 0.000000000000000000, 0.000000000000000000, 1.000000000000000000 ) ) ;
#14450 = DIRECTION ( 'NONE',  ( 0.000000000000000000, 0.000000000000000000, 1.000000000000000000 ) ) ;
#14451 = ORIENTED_EDGE ( 'NONE', *, *, #26649, .F. ) ;
#14452 = CARTESIAN_POINT ( 'NONE',  ( -0.6119360453657125554, 0.1072290460171901605, 0.09685039370078740717 ) ) ;
#14453 = ORIENTED_EDGE ( 'NONE', *, *, #7757, .T. ) ;
#14454 = CARTESIAN_POINT ( 'NONE',  ( 0.3175540113612289050, 0.1078280746903826914, 1.953740157480315043 ) ) ;
#14455 = CARTESIAN_POINT ( 'NONE',  ( -0.3121994997578409481, -0.4069448477569437284, -1.550196850393700920 ) ) ;
#14456 = AXIS2_PLACEMENT_3D ( 'NONE', #11294, #15949, #7192 ) ;
#14457 = CARTESIAN_POINT ( 'NONE',  ( 0.000000000000000000, 0.5905511811023621549, -0.4921259842519685179 ) ) ;
#14458 = CIRCLE ( 'NONE', #7688, 0.2362204724225640262 ) ;
#14459 = CARTESIAN_POINT ( 'NONE',  ( -0.5526079293737016229, 0.1480156394741962422, 0.9399606299212598381 ) ) ;
#14460 = CARTESIAN_POINT ( 'NONE',  ( 0.000000000000000000, 0.9055118110236221041, 0.000000000000000000 ) ) ;
#14461 = DIRECTION ( 'NONE',  ( 0.000000000000000000, -1.000000000000000000, 0.000000000000000000 ) ) ;
#14462 = ORIENTED_EDGE ( 'NONE', *, *, #10333, .T. ) ;
#14463 = DIRECTION ( 'NONE',  ( 0.000000000000000000, 0.000000000000000000, -1.000000000000000000 ) ) ;
#14464 = TOROIDAL_SURFACE ( 'NONE', #26606, 0.6102362204724409711, 0.1299212598425196763 ) ;
#14465 = ORIENTED_EDGE ( 'NONE', *, *, #10225, .F. ) ;
#14466 = CARTESIAN_POINT ( 'NONE',  ( -0.4004902621171045896, 0.3511566718596346726, 1.747047244094488194 ) ) ;
#14467 = VERTEX_POINT ( 'NONE', #4978 ) ;
#14468 = CARTESIAN_POINT ( 'NONE',  ( -0.002724751885584056257, 0.1704774416898501010, 0.09842519685039388677 ) ) ;
#14469 = DIRECTION ( 'NONE',  ( -1.000000000000000000, 0.000000000000000000, 0.000000000000000000 ) ) ;
#14470 = CARTESIAN_POINT ( 'NONE',  ( 0.3584231247409862542, 4.389417324544413085E-17, -0.05511811023622047168 ) ) ;
#14471 = ORIENTED_EDGE ( 'NONE', *, *, #901, .T. ) ;
#14472 = EDGE_CURVE ( 'NONE', #20206, #24622, #24997, .T. ) ;
#14473 = CARTESIAN_POINT ( 'NONE',  ( -0.5640458768698323189, -0.5269038574489980364, 0.9872771499275302398 ) ) ;
#14474 = VERTEX_POINT ( 'NONE', #482 ) ;
#14475 = CARTESIAN_POINT ( 'NONE',  ( -0.6996455634084097763, -0.1588938903144868908, 0.1601585119419891567 ) ) ;
#14476 = DIRECTION ( 'NONE',  ( 1.000000000000000000, 0.000000000000000000, 0.000000000000000000 ) ) ;
#14477 = AXIS2_PLACEMENT_3D ( 'NONE', #2637, #24387, #9398 ) ;
#14478 = DIRECTION ( 'NONE',  ( -0.000000000000000000, -1.000000000000000000, -0.000000000000000000 ) ) ;
#14479 = CARTESIAN_POINT ( 'NONE',  ( -0.5751347059550788732, -0.6192722590600424626, -0.9188490092315169111 ) ) ;
#14480 = CARTESIAN_POINT ( 'NONE',  ( 0.4067073728345488304, -0.2341441294389854655, 0.07637795275590551769 ) ) ;
#14481 = CARTESIAN_POINT ( 'NONE',  ( 0.1512365701434774945, 0.2025839336325081785, 0.4452122039724091263 ) ) ;
#14482 = CARTESIAN_POINT ( 'NONE',  ( -0.1968503937007874127, 0.000000000000000000, 0.09092130223458683158 ) ) ;
#14483 = ORIENTED_EDGE ( 'NONE', *, *, #12450, .F. ) ;
#14484 = DIRECTION ( 'NONE',  ( 0.000000000000000000, 0.000000000000000000, 1.000000000000000000 ) ) ;
#14485 = CARTESIAN_POINT ( 'NONE',  ( -0.3149606299212598381, 0.000000000000000000, 0.000000000000000000 ) ) ;
#14486 = AXIS2_PLACEMENT_3D ( 'NONE', #25169, #27301, #3696 ) ;
#14487 = FACE_OUTER_BOUND ( 'NONE', #8451, .T. ) ;
#14488 = ORIENTED_EDGE ( 'NONE', *, *, #26400, .T. ) ;
#14489 = CARTESIAN_POINT ( 'NONE',  ( 0.02345921195929052613, -0.3574961452116294791, -3.115157480314960647 ) ) ;
#14490 = PRODUCT_DEFINITION_CONTEXT ( 'detailed design', #20452, 'design' ) ;
#14491 = ORIENTED_EDGE ( 'NONE', *, *, #14302, .F. ) ;
#14492 = CARTESIAN_POINT ( 'NONE',  ( 0.3996230174612964148, -0.1970259548082136380, -1.934055118110236338 ) ) ;
#14493 = B_SPLINE_CURVE_WITH_KNOTS ( 'NONE', 3,
 ( #27487, #27769, #12778, #3888, #8274, #15195 ),
 .UNSPECIFIED., .F., .F.,
 ( 4, 2, 4 ),
 ( 0.5000000000000000000, 0.7500000000000000000, 1.000000000000000000 ),
 .UNSPECIFIED. ) ;
#14494 = EDGE_CURVE ( 'NONE', #12596, #3390, #13602, .T. ) ;
#14495 = ADVANCED_FACE ( 'NONE', ( #4834, #895 ), #9203, .T. ) ;
#14496 = AXIS2_PLACEMENT_3D ( 'NONE', #25929, #256, #6440 ) ;
#14497 = ORIENTED_EDGE ( 'NONE', *, *, #838, .T. ) ;
#14498 = ORIENTED_EDGE ( 'NONE', *, *, #15042, .F. ) ;
#14499 = VERTEX_POINT ( 'NONE', #17944 ) ;
#14501 = CARTESIAN_POINT ( 'NONE',  ( -0.5833277509429386498, -0.1953566107329901547, -0.09839827897590196215 ) ) ;
#14502 = ( NAMED_UNIT ( * ) PLANE_ANGLE_UNIT ( ) SI_UNIT ( $, .RADIAN. ) ) ;
#14503 = CARTESIAN_POINT ( 'NONE',  ( 0.4004221243553300891, 0.3512268162760394108, 1.747047244094488194 ) ) ;
#14504 = EDGE_CURVE ( 'NONE', #88, #7980, #16977, .T. ) ;
#14505 = LINE ( 'NONE', #7851, #8003 ) ;
#14506 = ORIENTED_EDGE ( 'NONE', *, *, #22356, .T. ) ;
#14507 = AXIS2_PLACEMENT_3D ( 'NONE', #8573, #8841, #15224 ) ;
#14508 = CARTESIAN_POINT ( 'NONE',  ( 0.3644697409450285974, -0.09762295995069371346, -3.100567304031760951 ) ) ;
#14509 = EDGE_CURVE ( 'NONE', #11779, #5913, #6834, .T. ) ;
#14510 = CARTESIAN_POINT ( 'NONE',  ( -0.02325127328526653894, -0.3543321272855305404, 1.953740157480315043 ) ) ;
#14511 = CARTESIAN_POINT ( 'NONE',  ( 0.3020979083623086536, 0.3591256245825952265, 0.1992125984251968684 ) ) ;
#14512 = CARTESIAN_POINT ( 'NONE',  ( 0.04115487667019134682, -0.5425147539706086652, -0.05108106348549787401 ) ) ;
#14513 = CARTESIAN_POINT ( 'NONE',  ( 0.2161381151963047975, 0.2817310484609297228, 1.953740157480315043 ) ) ;
#14514 = EDGE_LOOP ( 'NONE', ( #23123, #11587, #22975, #21753 ) ) ;
#14515 = CARTESIAN_POINT ( 'NONE',  ( -0.6187410091539320423, -0.08521673449347196005, -0.2406752346771077189 ) ) ;
#14517 = CARTESIAN_POINT ( 'NONE',  ( 0.3772436174784756235, 0.4300830224589536899, 0.9399606299212598381 ) ) ;
#14516 = CARTESIAN_POINT ( 'NONE',  ( -0.04928528614549732706, -0.3765118517642104257, -3.100567304031763616 ) ) ;
#14518 = B_SPLINE_CURVE_WITH_KNOTS ( 'NONE', 3,
 ( #23281, #3909, #20586, #1241 ),
 .UNSPECIFIED., .F., .F.,
 ( 4, 4 ),
 ( 1.006307675027575899, 1.007953978091874037 ),
 .UNSPECIFIED. ) ;
#14519 = ORIENTED_EDGE ( 'NONE', *, *, #20478, .T. ) ;
#14520 = ORIENTED_EDGE ( 'NONE', *, *, #14920, .T. ) ;
#14521 = DIRECTION ( 'NONE',  ( 0.000000000000000000, 0.000000000000000000, 1.000000000000000000 ) ) ;
#14522 = CARTESIAN_POINT ( 'NONE',  ( 0.000000000000000000, 0.000000000000000000, -4.330708661417323135 ) ) ;
#14523 = VECTOR ( 'NONE', #18254, 39.37007874015748143 ) ;
#14525 = CARTESIAN_POINT ( 'NONE',  ( 0.3574975638436101444, -0.02339816079119092299, -3.115157480314960647 ) ) ;
#14526 = CARTESIAN_POINT ( 'NONE',  ( 0.5511811023622046335, -0.07214943758244278527, 0.9202755905511811330 ) ) ;
#14527 = CARTESIAN_POINT ( 'NONE',  ( 0.000000000000000000, 0.000000000000000000, -0.05856299212598425896 ) ) ;
#14528 = DIRECTION ( 'NONE',  ( 1.000000000000000000, 0.000000000000000000, 0.000000000000000000 ) ) ;
#14529 = CIRCLE ( 'NONE', #2310, 0.4692913385826771866 ) ;
#14530 = DIRECTION ( 'NONE',  ( 0.000000000000000000, 0.000000000000000000, 1.000000000000000000 ) ) ;
#14531 = AXIS2_PLACEMENT_3D ( 'NONE', #26912, #13921, #11941 ) ;
#14532 = CARTESIAN_POINT ( 'NONE',  ( 1.857656692913385893E-16, -6.267877317605309469E-17, -0.5118110235513823048 ) ) ;
#14533 = DIRECTION ( 'NONE',  ( 1.000000000000000000, 0.000000000000000000, 0.000000000000000000 ) ) ;
#14534 = VERTEX_POINT ( 'NONE', #19958 ) ;
#14535 = DIRECTION ( 'NONE',  ( 0.000000000000000000, 0.000000000000000000, 1.000000000000000000 ) ) ;
#14536 = CARTESIAN_POINT ( 'NONE',  ( 0.4848217985909654137, 5.937354638012884952E-17, -0.05511811023622047168 ) ) ;
#14537 = DIRECTION ( 'NONE',  ( 0.000000000000000000, 0.000000000000000000, 1.000000000000000000 ) ) ;
#14538 = DIRECTION ( 'NONE',  ( -0.2036417511401760472, -0.9790454724845840673, 0.000000000000000000 ) ) ;
#14539 = EDGE_CURVE ( 'NONE', #3868, #27722, #10684, .T. ) ;
#14540 = CARTESIAN_POINT ( 'NONE',  ( 0.6882266799383695011, -0.4143730867902977177, 0.1723141108463512317 ) ) ;
#14541 = CARTESIAN_POINT ( 'NONE',  ( -0.03478633594543645985, -0.5314960629921260393, 1.747047244094488194 ) ) ;
#14542 = ( REPRESENTATION_RELATIONSHIP ('NONE','NONE', #12434, #26684 ) REPRESENTATION_RELATIONSHIP_WITH_TRANSFORMATION ( #13251 )SHAPE_REPRESENTATION_RELATIONSHIP( ) ) ;
#14543 = FACE_OUTER_BOUND ( 'NONE', #455, .T. ) ;
#14544 = FACE_OUTER_BOUND ( 'NONE', #5982, .T. ) ;
#14545 = EDGE_CURVE ( 'NONE', #15551, #17891, #2159, .T. ) ;
#14546 = CARTESIAN_POINT ( 'NONE',  ( -0.4441657790107740866, 0.2564944395515753039, 1.766732283464566899 ) ) ;
#14547 = ORIENTED_EDGE ( 'NONE', *, *, #2115, .T. ) ;
#14548 = AXIS2_PLACEMENT_3D ( 'NONE', #2561, #13036, #19808 ) ;
#14549 = EDGE_LOOP ( 'NONE', ( #9853, #4271, #2257, #3276 ) ) ;
#14550 = CARTESIAN_POINT ( 'NONE',  ( -0.1584254766472275311, 0.3213305936751604253, -3.115157480314960647 ) ) ;
#14551 = VERTEX_POINT ( 'NONE', #17188 ) ;
#14553 = EDGE_CURVE ( 'NONE', #24778, #1564, #9540, .T. ) ;
#14552 = CARTESIAN_POINT ( 'NONE',  ( -0.1574803149606299191, 0.000000000000000000, 0.000000000000000000 ) ) ;
#14554 = CARTESIAN_POINT ( 'NONE',  ( -0.1694923354753281042, -0.4674199084430591400, 0.1140743250961406413 ) ) ;
#14555 = CARTESIAN_POINT ( 'NONE',  ( -2.048885995248197414E-16, 2.509161675898543984E-32, 0.5532930914870255457 ) ) ;
#14556 = CARTESIAN_POINT ( 'NONE',  ( 0.2211428102655756955, 0.2521176338356569957, 1.973425196850393970 ) ) ;
#14557 = ORIENTED_EDGE ( 'NONE', *, *, #1228, .F. ) ;
#14558 = ORIENTED_EDGE ( 'NONE', *, *, #11263, .T. ) ;
#14559 = B_SPLINE_CURVE_WITH_KNOTS ( 'NONE', 3,
 ( #15352, #25922, #21689, #13339 ),
 .UNSPECIFIED., .F., .F.,
 ( 4, 4 ),
 ( 0.6915327610580708217, 0.6928470748408740443 ),
 .UNSPECIFIED. ) ;
#14560 = CARTESIAN_POINT ( 'NONE',  ( -0.2466292688015021273, -0.4270824798167794922, -1.550196850393700920 ) ) ;
#14561 = CARTESIAN_POINT ( 'NONE',  ( -0.4055307389460929279, 0.000000000000000000, -0.1111195235210984261 ) ) ;
#14562 = CARTESIAN_POINT ( 'NONE',  ( -0.5708661417322834497, 0.000000000000000000, 0.9399606299212598381 ) ) ;
#14563 = ORIENTED_EDGE ( 'NONE', *, *, #14539, .T. ) ;
#14564 = CONTEXT_DEPENDENT_SHAPE_REPRESENTATION ( #14148, #22009 ) ;
#14565 = FACE_OUTER_BOUND ( 'NONE', #7726, .T. ) ;
#14566 = CARTESIAN_POINT ( 'NONE',  ( 0.000000000000000000, 0.4724409448818898127, 0.000000000000000000 ) ) ;
#14567 = CARTESIAN_POINT ( 'NONE',  ( 0.4790936880894704486, 0.08507591033005897085, 0.09284957166276250340 ) ) ;
#14568 = PRODUCT ( 'Cam Shaft', 'Cam Shaft', '', ( #2483 ) ) ;
#14569 = VECTOR ( 'NONE', #12546, 39.37007874015748143 ) ;
#14570 = CIRCLE ( 'NONE', #2344, 0.3149606299212598381 ) ;
#14571 = EDGE_LOOP ( 'NONE', ( #18166, #10213, #14640, #24438, #2254 ) ) ;
#14572 = CARTESIAN_POINT ( 'NONE',  ( -0.4029514798600966063, 0.3205030004496360330, 0.3251195115602828478 ) ) ;
#14573 = CARTESIAN_POINT ( 'NONE',  ( 0.1490609433576163545, -0.2393035190829114200, 0.4144858534816307505 ) ) ;
#14574 = CARTESIAN_POINT ( 'NONE',  ( 0.1259842519685039353, 4.470295275590551256E-17, -8.195543307086614694E-17 ) ) ;
#14575 = DIRECTION ( 'NONE',  ( 0.000000000000000000, 0.000000000000000000, 1.000000000000000000 ) ) ;
#14576 = CIRCLE ( 'NONE', #11370, 0.5379714048901780288 ) ;
#14577 = CARTESIAN_POINT ( 'NONE',  ( -0.5885963067485330269, -0.2400798436957021775, 0.2138130534390355331 ) ) ;
#14578 = CARTESIAN_POINT ( 'NONE',  ( 0.1599629598573263645, -0.4411872753632007926, 0.1992125984251968684 ) ) ;
#14579 = DIRECTION ( 'NONE',  ( -0.4999999999999997780, 0.8660254037844388186, 0.000000000000000000 ) ) ;
#14580 = DIRECTION ( 'NONE',  ( 0.000000000000000000, 1.000000000000000000, 0.000000000000000000 ) ) ;
#14581 = EDGE_CURVE ( 'NONE', #18025, #7189, #14992, .T. ) ;
#14582 = CARTESIAN_POINT ( 'NONE',  ( 8.810208661417323492E-17, -4.420669291338583154E-18, 0.000000000000000000 ) ) ;
#14583 = VERTEX_POINT ( 'NONE', #5697 ) ;
#14584 = ORIENTED_EDGE ( 'NONE', *, *, #12822, .F. ) ;
#14585 = EDGE_CURVE ( 'NONE', #17275, #16783, #25168, .T. ) ;
#14586 = VERTEX_POINT ( 'NONE', #20939 ) ;
#14587 = AXIS2_PLACEMENT_3D ( 'NONE', #27466, #14913, #27753 ) ;
#14588 = DIRECTION ( 'NONE',  ( 0.000000000000000000, 0.000000000000000000, 1.000000000000000000 ) ) ;
#14589 = CARTESIAN_POINT ( 'NONE',  ( -0.2762247810519002922, 0.4783323773986519201, 0.9202755905511811330 ) ) ;
#14590 = VERTEX_POINT ( 'NONE', #22497 ) ;
#14591 = CARTESIAN_POINT ( 'NONE',  ( -1.692913385826771533, 0.07874015748031491790, -1.036610629921259805E-16 ) ) ;
#14592 = VERTEX_POINT ( 'NONE', #14025 ) ;
#14593 = AXIS2_PLACEMENT_3D ( 'NONE', #11305, #13291, #24294 ) ;
#14594 = CARTESIAN_POINT ( 'NONE',  ( 0.000000000000000000, 0.000000000000000000, 0.2637795275590551491 ) ) ;
#14595 = DIRECTION ( 'NONE',  ( 0.000000000000000000, -1.000000000000000000, 0.000000000000000000 ) ) ;
#14596 = DIRECTION ( 'NONE',  ( 3.508907999999999048E-18, -0.4999999999999998890, 0.8660254037844388186 ) ) ;
#14597 = CARTESIAN_POINT ( 'NONE',  ( 0.1707210962531913734, -0.4707890492249701131, 0.09685039370078740717 ) ) ;
#14598 = VERTEX_POINT ( 'NONE', #18518 ) ;
#14599 = CARTESIAN_POINT ( 'NONE',  ( -0.1658556822965989719, -0.4573967274740618483, 0.1075369453282564308 ) ) ;
#14600 = CARTESIAN_POINT ( 'NONE',  ( 0.5118110236220473341, 6.402768735150616610E-17, -1.550196850393700920 ) ) ;
#14601 = CARTESIAN_POINT ( 'NONE',  ( 0.3382184156748877513, 0.3855916753034390188, -1.550196850393700920 ) ) ;
#14602 = AXIS2_PLACEMENT_3D ( 'NONE', #6475, #12959, #15241 ) ;
#14603 = ( BOUNDED_CURVE ( )  B_SPLINE_CURVE ( 2, ( #10587, #17011, #4434 ),
 .UNSPECIFIED., .F., .F. ) 
 B_SPLINE_CURVE_WITH_KNOTS ( ( 3, 3 ),
 ( 0.000000000000000000, 0.5842180690389588982 ),
 .UNSPECIFIED. ) 
 CURVE ( )  GEOMETRIC_REPRESENTATION_ITEM ( )  RATIONAL_B_SPLINE_CURVE ( ( 1.000000000000000000, 1.154700538379251906, 1.000000000000000000 ) ) 
 REPRESENTATION_ITEM ( '' )  ) ;
#14604 = CARTESIAN_POINT ( 'NONE',  ( 0.05938807134538631044, -0.05663358325667527254, -0.4684893292439904489 ) ) ;
#14605 = EDGE_CURVE ( 'NONE', #20499, #21578, #22925, .T. ) ;
#14606 = CIRCLE ( 'NONE', #20439, 0.6299212598425196763 ) ;
#14607 = B_SPLINE_CURVE_WITH_KNOTS ( 'NONE', 3,
 ( #10317, #6109, #14746, #21210 ),
 .UNSPECIFIED., .F., .F.,
 ( 4, 4 ),
 ( 1.164573402063411978, 1.166266105206986037 ),
 .UNSPECIFIED. ) ;
#14608 = CARTESIAN_POINT ( 'NONE',  ( 0.4152525734085952824, 0.3642352168757231889, 0.9399606299212598381 ) ) ;
#14609 = CARTESIAN_POINT ( 'NONE',  ( 0.1918813796216842782, -0.5271897577243779276, 0.1771653543307086520 ) ) ;
#14610 = EDGE_LOOP ( 'NONE', ( #11240, #16108, #14519, #17680 ) ) ;
#14611 = CARTESIAN_POINT ( 'NONE',  ( -0.3392608232658738676, 0.1151343661288097980, -3.115157480314960647 ) ) ;
#14612 = EDGE_CURVE ( 'NONE', #607, #22369, #7853, .T. ) ;
#14613 = AXIS2_PLACEMENT_3D ( 'NONE', #24852, #24427, #27827 ) ;
#14614 = ( LENGTH_UNIT ( ) NAMED_UNIT ( * ) SI_UNIT ( $, .METRE. ) ) ;
#14615 = ORIENTED_EDGE ( 'NONE', *, *, #18002, .T. ) ;
#14616 = VECTOR ( 'NONE', #23322, 39.37007874015748143 ) ;
#14617 = B_SPLINE_CURVE_WITH_KNOTS ( 'NONE', 3,
 ( #11402, #13657, #9403, #22276, #22140, #15922, #674, #26646, #17878, #9264, #7167, #2908, #7587, #6043, #11967, #1785, #9840, #18440 ),
 .UNSPECIFIED., .F., .F.,
 ( 4, 2, 2, 2, 2, 2, 2, 2, 4 ),
 ( 0.000000000000000000, 0.1250000000000000000, 0.2500000000000000000, 0.3750000000000000000, 0.5000000000000000000, 0.6250000000000000000, 0.7500000000000000000, 0.8750000000000000000, 1.000000000000000000 ),
 .UNSPECIFIED. ) ;
#14618 = ORIENTED_EDGE ( 'NONE', *, *, #23655, .T. ) ;
#14619 = CARTESIAN_POINT ( 'NONE',  ( -0.06699507805604322519, 0.5085118447796660446, -1.550196850393700920 ) ) ;
#14620 = ORIENTED_EDGE ( 'NONE', *, *, #24469, .F. ) ;
#14621 = CARTESIAN_POINT ( 'NONE',  ( -1.355511558298621910, 1.564461769117756029, 1.633858267716535639 ) ) ;
#14622 = PLANE ( 'NONE',  #19225 ) ;
#14623 = DIRECTION ( 'NONE',  ( 0.000000000000000000, 0.000000000000000000, 1.000000000000000000 ) ) ;
#14624 = DIRECTION ( 'NONE',  ( -1.000000000000000000, 0.000000000000000000, 0.000000000000000000 ) ) ;
#14625 = EDGE_LOOP ( 'NONE', ( #23943, #15268 ) ) ;
#14626 = TOROIDAL_SURFACE ( 'NONE', #13673, 0.6102362204724409711, 0.1299212598425196763 ) ;
#14627 = CARTESIAN_POINT ( 'NONE',  ( -0.0006679551606482677165, 0.5322830454629158270, 0.1322834645669291320 ) ) ;
#14628 = ORIENTED_EDGE ( 'NONE', *, *, #13073, .T. ) ;
#14629 = EDGE_CURVE ( 'NONE', #25578, #5717, #7873, .T. ) ;
#14630 = AXIS2_PLACEMENT_3D ( 'NONE', #11385, #13366, #17863 ) ;
#14631 = DIRECTION ( 'NONE',  ( -1.000000000000000000, 0.000000000000000000, 0.000000000000000000 ) ) ;
#14632 = CARTESIAN_POINT ( 'NONE',  ( 0.3018020646414338870, 0.3593743330771607125, 0.07637549214372835182 ) ) ;
#14633 = DIRECTION ( 'NONE',  ( 0.000000000000000000, 0.000000000000000000, -1.000000000000000000 ) ) ;
#14634 = CARTESIAN_POINT ( 'NONE',  ( 0.2104048168833876076, -0.4354435989199126888, 0.2715646632207475708 ) ) ;
#14635 = ORIENTED_EDGE ( 'NONE', *, *, #13203, .F. ) ;
#14636 = DIRECTION ( 'NONE',  ( 1.000000000000000000, 0.000000000000000000, 0.000000000000000000 ) ) ;
#14637 = CONICAL_SURFACE ( 'NONE', #2413, 0.4526932812344527379, 0.1178097243749990780 ) ;
#14638 = CARTESIAN_POINT ( 'NONE',  ( 0.7874015748031496509, 0.000000000000000000, -1.052618110236220428 ) ) ;
#14639 = VECTOR ( 'NONE', #9933, 39.37007874015748854 ) ;
#14640 = ORIENTED_EDGE ( 'NONE', *, *, #13114, .T. ) ;
#14641 = CARTESIAN_POINT ( 'NONE',  ( 0.04673614183192328908, -0.3552064049865930051, -3.115157480314960203 ) ) ;
#14642 = CARTESIAN_POINT ( 'NONE',  ( -0.1173917140416368271, -0.4382752542996092293, -1.934055118110236338 ) ) ;
#14643 = CARTESIAN_POINT ( 'NONE',  ( 0.4555658499975999698, -0.06001958459475366381, -1.928289503579165398 ) ) ;
#14644 = EDGE_CURVE ( 'NONE', #12919, #6711, #20935, .T. ) ;
#14645 = AXIS2_PLACEMENT_3D ( 'NONE', #17262, #10901, #206 ) ;
#14646 = VERTEX_POINT ( 'NONE', #14310 ) ;
#14647 = CARTESIAN_POINT ( 'NONE',  ( -0.4881018399981850719, -0.3837266214674216469, -0.3317898348603995351 ) ) ;
#14648 = DIRECTION ( 'NONE',  ( -0.000000000000000000, -1.000000000000000000, -0.000000000000000000 ) ) ;
#14649 = CARTESIAN_POINT ( 'NONE',  ( -0.4612490782034870396, -0.2663596103035605345, 1.747047244094488194 ) ) ;
#14650 = EDGE_LOOP ( 'NONE', ( #9966, #10084 ) ) ;
#14651 = ( CONVERSION_BASED_UNIT ( 'INCH', #16739 ) LENGTH_UNIT ( ) NAMED_UNIT ( #7979 ) ) ;
#14652 = AXIS2_PLACEMENT_3D ( 'NONE', #15305, #15698, #26547 ) ;
#14653 = CARTESIAN_POINT ( 'NONE',  ( -0.3937007874015748254, 0.000000000000000000, 0.000000000000000000 ) ) ;
#14654 = AXIS2_PLACEMENT_3D ( 'NONE', #15300, #12633, #1894 ) ;
#14655 = CARTESIAN_POINT ( 'NONE',  ( -0.03532354024591901481, -0.8267716535433071723, 0.000000000000000000 ) ) ;
#14656 = CARTESIAN_POINT ( 'NONE',  ( 0.02917857698688243462, 0.4446035140077004844, -1.934055118110236338 ) ) ;
#14657 = CARTESIAN_POINT ( 'NONE',  ( 0.2341512108694336625, 0.2669480828848126985, 1.953740157480315043 ) ) ;
#14658 = ORIENTED_EDGE ( 'NONE', *, *, #25561, .T. ) ;
#14659 = VERTEX_POINT ( 'NONE', #18660 ) ;
#14660 = DIRECTION ( 'NONE',  ( 0.000000000000000000, 1.000000000000000000, 0.000000000000000000 ) ) ;
#14661 = CARTESIAN_POINT ( 'NONE',  ( 0.000000000000000000, 0.000000000000000000, 0.2755905511811023723 ) ) ;
#14663 = CARTESIAN_POINT ( 'NONE',  ( 0.4539000224941021067, -0.3482225189666773302, 0.9399606299212598381 ) ) ;
#14662 = LINE ( 'NONE', #5891, #8599 ) ;
#14664 = ORIENTED_EDGE ( 'NONE', *, *, #10616, .T. ) ;
#14665 = ORIENTED_EDGE ( 'NONE', *, *, #23833, .F. ) ;
#14666 = DIRECTION ( 'NONE',  ( -1.000000000000000000, 0.000000000000000000, 0.000000000000000000 ) ) ;
#14667 = DIRECTION ( 'NONE',  ( -1.000000000000000000, 0.000000000000000000, 0.000000000000000000 ) ) ;
#14668 = AXIS2_PLACEMENT_3D ( 'NONE', #23179, #1690, #12432 ) ;
#14669 = EDGE_CURVE ( 'NONE', #27454, #18611, #9189, .T. ) ;
#14670 = CARTESIAN_POINT ( 'NONE',  ( 0.3392387706403792169, -0.1151913129404410208, -3.115157480314960647 ) ) ;
#14671 = CARTESIAN_POINT ( 'NONE',  ( 0.3387265385688508768, -0.4407612517155324316, 0.9202755905511812440 ) ) ;
#14672 = DIRECTION ( 'NONE',  ( 1.000000000000000000, 0.000000000000000000, 0.000000000000000000 ) ) ;
#14673 = CARTESIAN_POINT ( 'NONE',  ( 0.4535326485287339282, 0.08054850140356757671, 0.1771653543307084855 ) ) ;
#14674 = CARTESIAN_POINT ( 'NONE',  ( -1.197070535079588716, 0.07874015748031495954, -1.197070535079588716 ) ) ;
#14675 = AXIS2_PLACEMENT_3D ( 'NONE', #14429, #11724, #18200 ) ;
#14676 = EDGE_CURVE ( 'NONE', #14016, #6594, #27255, .T. ) ;
#14677 = CARTESIAN_POINT ( 'NONE',  ( 0.0006832381873096096290, 0.6614169699447792761, 0.1926811207755882993 ) ) ;
#14678 = VERTEX_POINT ( 'NONE', #12319 ) ;
#14679 = CARTESIAN_POINT ( 'NONE',  ( -0.4954757973260912052, 0.2860025288262565413, 0.9399606299212600602 ) ) ;
#14680 = FACE_OUTER_BOUND ( 'NONE', #23535, .T. ) ;
#14681 = DIRECTION ( 'NONE',  ( -1.000000000000000000, 0.000000000000000000, 0.000000000000000000 ) ) ;
#14682 = ORIENTED_EDGE ( 'NONE', *, *, #14893, .T. ) ;
#14683 = ORIENTED_EDGE ( 'NONE', *, *, #18215, .T. ) ;
#14684 = VERTEX_POINT ( 'NONE', #24600 ) ;
#14685 = DIRECTION ( 'NONE',  ( 0.000000000000000000, 1.000000000000000000, 0.000000000000000000 ) ) ;
#14686 = CARTESIAN_POINT ( 'NONE',  ( 0.4225965726693019509, -0.3242071728275352505, 1.747047244094488194 ) ) ;
#14687 = CARTESIAN_POINT ( 'NONE',  ( -0.2256062985780004637, -0.6178563876545716260, 0.1461456498321150876 ) ) ;
#14688 = CARTESIAN_POINT ( 'NONE',  ( 0.5085118447801426633, -0.06699507805369582514, 1.766732283464566899 ) ) ;
#14689 = CIRCLE ( 'NONE', #8803, 0.07677362204724409722 ) ;
#14690 = ORIENTED_EDGE ( 'NONE', *, *, #20264, .T. ) ;
#14691 = ORIENTED_EDGE ( 'NONE', *, *, #22328, .T. ) ;
#14692 = CARTESIAN_POINT ( 'NONE',  ( -0.1584254766472190379, -0.3213305936751582048, -3.115157480314960647 ) ) ;
#14693 = ORIENTED_EDGE ( 'NONE', *, *, #2713, .T. ) ;
#14694 = CARTESIAN_POINT ( 'NONE',  ( 0.06002032661671147240, -0.4585215200179057482, -1.928289503579156516 ) ) ;
#14695 = SHAPE_REPRESENTATION_RELATIONSHIP ( 'NONE' , 'NONE' ,  #5415, #17421 ) ;
#14696 = CARTESIAN_POINT ( 'NONE',  ( -0.4986013261500205074, 0.000000000000000000, -0.2204724409448818867 ) ) ;
#14697 = CARTESIAN_POINT ( 'NONE',  ( -0.2521176338356572177, -0.2211428102655754180, 1.973425196850393970 ) ) ;
#14698 = ORIENTED_EDGE ( 'NONE', *, *, #20353, .T. ) ;
#14699 = ORIENTED_EDGE ( 'NONE', *, *, #26922, .F. ) ;
#14700 = CONICAL_SURFACE ( 'NONE', #684, 0.3224687058348476576, 0.8056700744428512140 ) ;
#14701 = EDGE_CURVE ( 'NONE', #5816, #27022, #22774, .T. ) ;
#14702 = CARTESIAN_POINT ( 'NONE',  ( 0.2466292688015071233, 0.4270824798167958125, -1.550196850393700920 ) ) ;
#14703 = DIRECTION ( 'NONE',  ( 0.000000000000000000, -1.000000000000000000, 0.000000000000000000 ) ) ;
#14704 = PLANE ( 'NONE',  #9148 ) ;
#14705 = AXIS2_PLACEMENT_3D ( 'NONE', #3905, #14672, #12799 ) ;
#14706 = ORIENTED_EDGE ( 'NONE', *, *, #3995, .F. ) ;
#14707 = ORIENTED_EDGE ( 'NONE', *, *, #5679, .F. ) ;
#14708 = EDGE_CURVE ( 'NONE', #6078, #3924, #27726, .T. ) ;
#14709 = CYLINDRICAL_SURFACE ( 'NONE', #27541, 0.1771653543307086520 ) ;
#14710 = CARTESIAN_POINT ( 'NONE',  ( -0.0005710523241074312757, 0.4632828964890012835, 0.2048502514557469789 ) ) ;
#14711 = DIRECTION ( 'NONE',  ( 0.000000000000000000, 0.000000000000000000, 1.000000000000000000 ) ) ;
#14712 = CARTESIAN_POINT ( 'NONE',  ( 0.4922996667773191226, 0.08741303158496288583, 0.1496602734591142292 ) ) ;
#14713 = VERTEX_POINT ( 'NONE', #10186 ) ;
#14714 = EDGE_CURVE ( 'NONE', #5717, #25431, #13260, .T. ) ;
#14715 = CONICAL_SURFACE ( 'NONE', #7925, 0.1106489370078739681, 0.08726646250000029414 ) ;
#14716 = EDGE_LOOP ( 'NONE', ( #24966, #25552, #7561, #8706, #23121, #13748 ) ) ;
#14717 = LINE ( 'NONE', #12134, #14616 ) ;
#14718 = EDGE_CURVE ( 'NONE', #10159, #27805, #23208, .T. ) ;
#14719 = B_SPLINE_CURVE_WITH_KNOTS ( 'NONE', 3,
 ( #24168, #17793, #20199, #15826, #2952, #22461 ),
 .UNSPECIFIED., .F., .F.,
 ( 4, 2, 4 ),
 ( 0.5000000000000000000, 0.7500000000000000000, 1.000000000000000000 ),
 .UNSPECIFIED. ) ;
#14720 = APPLICATION_CONTEXT ( 'automotive_design' ) ;
#14721 = CARTESIAN_POINT ( 'NONE',  ( 0.4692913385826771866, 0.000000000000000000, 0.07637795275590551769 ) ) ;
#14722 = DIRECTION ( 'NONE',  ( 1.000000000000000000, 0.000000000000000000, 0.000000000000000000 ) ) ;
#14723 = DIRECTION ( 'NONE',  ( 0.000000000000000000, 0.000000000000000000, 1.000000000000000000 ) ) ;
#14724 = AXIS2_PLACEMENT_3D ( 'NONE', #10065, #18671, #8105 ) ;
#14725 = CARTESIAN_POINT ( 'NONE',  ( -0.5943649339014159816, -0.2199389736434831377, 0.2173156648486553322 ) ) ;
#14726 = CARTESIAN_POINT ( 'NONE',  ( -0.4622619257814346572, 0.08092139668567638333, 0.07637795275590551769 ) ) ;
#14727 = CIRCLE ( 'NONE', #2038, 0.3937007873768824662 ) ;
#14728 = LINE ( 'NONE', #16955, #654 ) ;
#14729 = CARTESIAN_POINT ( 'NONE',  ( -0.0005939837304750000086, 0.5007870493127504208, 0.2574803149606298969 ) ) ;
#14730 = DIRECTION ( 'NONE',  ( -1.000000000000000000, 0.000000000000000000, 0.000000000000000000 ) ) ;
#14731 = EDGE_LOOP ( 'NONE', ( #13978, #11837 ) ) ;
#14732 = CARTESIAN_POINT ( 'NONE',  ( 0.3062557396297003187, -0.6341756901040335181, 0.1443310008622352147 ) ) ;
#14733 = DIRECTION ( 'NONE',  ( 0.000000000000000000, 0.000000000000000000, -1.000000000000000000 ) ) ;
#14734 = AXIS2_PLACEMENT_3D ( 'NONE', #8226, #4542, #8370 ) ;
#14735 = ORIENTED_EDGE ( 'NONE', *, *, #12634, .T. ) ;
#14736 = DIRECTION ( 'NONE',  ( 0.000000000000000000, 0.000000000000000000, 1.000000000000000000 ) ) ;
#14737 = DIRECTION ( 'NONE',  ( 0.000000000000000000, -1.000000000000000000, 0.000000000000000000 ) ) ;
#14738 = CARTESIAN_POINT ( 'NONE',  ( -0.07214854559198219386, 0.5476281405333177643, 0.9202755905511811330 ) ) ;
#14739 = EDGE_LOOP ( 'NONE', ( #14782, #4917, #18187, #19771 ) ) ;
#14740 = CARTESIAN_POINT ( 'NONE',  ( -0.3528204557971049149, 0.06272520244115065147, 0.1805249803441617285 ) ) ;
#14741 = DIRECTION ( 'NONE',  ( 0.000000000000000000, 1.000000000000000000, 0.000000000000000000 ) ) ;
#14742 = ORIENTED_EDGE ( 'NONE', *, *, #11304, .F. ) ;
#14743 = EDGE_CURVE ( 'NONE', #12366, #1421, #8566, .T. ) ;
#14744 = DIRECTION ( 'NONE',  ( 0.000000000000000000, 0.000000000000000000, 1.000000000000000000 ) ) ;
#14745 = CIRCLE ( 'NONE', #21471, 0.8267716535433071723 ) ;
#14746 = CARTESIAN_POINT ( 'NONE',  ( -0.0004447986960614961401, 0.5322833254990984031, 0.3401591244667909186 ) ) ;
#14747 = DIRECTION ( 'NONE',  ( 0.000000000000000000, 0.000000000000000000, 1.000000000000000000 ) ) ;
#14748 = EDGE_CURVE ( 'NONE', #12348, #18025, #3796, .T. ) ;
#14749 = CIRCLE ( 'NONE', #3880, 0.6614173228346456046 ) ;
#14750 = EDGE_LOOP ( 'NONE', ( #4164, #3891, #26702, #8266 ) ) ;
#14751 = DIRECTION ( 'NONE',  ( 1.000000000000000000, -1.147443000000000016E-15, 0.000000000000000000 ) ) ;
#14752 = EDGE_LOOP ( 'NONE', ( #3981, #1991, #9967, #22091 ) ) ;
#14753 = CARTESIAN_POINT ( 'NONE',  ( 0.3346456692913385988, 0.02190250779246873461, 1.953740157480315043 ) ) ;
#14754 = CARTESIAN_POINT ( 'NONE',  ( -0.03349795313024241800, -0.5118110236220473341, -1.550196850393700920 ) ) ;
#14755 = CARTESIAN_POINT ( 'NONE',  ( 0.06420467502049351238, -0.05385271582827236975, -0.4702630791244896691 ) ) ;
#14756 = CARTESIAN_POINT ( 'NONE',  ( -0.1429116519061139623, 0.5335524835332415838, 0.9399606299212598381 ) ) ;
#14757 = CARTESIAN_POINT ( 'NONE',  ( 0.2425693455392318731, 0.2888145544500153594, 0.1992150590373740204 ) ) ;
#14758 = DIRECTION ( 'NONE',  ( 0.000000000000000000, 0.000000000000000000, 1.000000000000000000 ) ) ;
#14759 = ORIENTED_EDGE ( 'NONE', *, *, #8608, .T. ) ;
#14760 = CARTESIAN_POINT ( 'NONE',  ( -0.3574975638436101999, 0.02346634615888416181, -3.115157480314961091 ) ) ;
#14761 = EDGE_CURVE ( 'NONE', #14847, #12355, #6072, .T. ) ;
#14762 = VERTEX_POINT ( 'NONE', #2277 ) ;
#14763 = TOROIDAL_SURFACE ( 'NONE', #8400, 0.5610236220472440971, 0.1003937007874015908 ) ;
#14764 = ORIENTED_EDGE ( 'NONE', *, *, #11596, .F. ) ;
#14765 = AXIS2_PLACEMENT_3D ( 'NONE', #16561, #10345, #27176 ) ;
#14766 = CARTESIAN_POINT ( 'NONE',  ( -0.5708661417322834497, 0.000000000000000000, 0.9399606299212598381 ) ) ;
#14767 = DIRECTION ( 'NONE',  ( -1.000000000000000000, 0.000000000000000000, 0.000000000000000000 ) ) ;
#14768 = CARTESIAN_POINT ( 'NONE',  ( -0.1187185187214592208, -0.3276343780106237280, 0.1589462317846821737 ) ) ;
#14769 = CARTESIAN_POINT ( 'NONE',  ( 0.5043865966252626398, -0.1711654737000346815, 1.747047244094488416 ) ) ;
#14770 = CARTESIAN_POINT ( 'NONE',  ( -0.1707210962531915677, -0.4707890492249701131, 0.09685039370078740717 ) ) ;
#14771 = EDGE_LOOP ( 'NONE', ( #7573, #1521 ) ) ;
#14772 = EDGE_CURVE ( 'NONE', #7184, #18835, #4268, .T. ) ;
#14773 = CARTESIAN_POINT ( 'NONE',  ( -0.6064065885002177803, -0.5142378326778294095, -0.9905099408302305841 ) ) ;
#14774 = CARTESIAN_POINT ( 'NONE',  ( -0.5704976599510874768, -0.5016113632412458889, -0.9930866184833081478 ) ) ;
#14775 = CARTESIAN_POINT ( 'NONE',  ( 0.2019525613798653363, -0.3664466487725785981, -0.6347042139374527991 ) ) ;
#14776 = CARTESIAN_POINT ( 'NONE',  ( -0.3412792617076848001, 0.05967164814832655317, 0.1276989850594592579 ) ) ;
#14777 = CARTESIAN_POINT ( 'NONE',  ( 0.2089723435111816296, -0.4324731448915267173, 0.2529987172005040974 ) ) ;
#14778 = EDGE_CURVE ( 'NONE', #25308, #12497, #21228, .T. ) ;
#14779 = ORIENTED_EDGE ( 'NONE', *, *, #2141, .T. ) ;
#14780 = DIRECTION ( 'NONE',  ( 0.000000000000000000, 1.000000000000000000, 0.000000000000000000 ) ) ;
#14781 = VECTOR ( 'NONE', #21277, 39.37007874015748854 ) ;
#14782 = ORIENTED_EDGE ( 'NONE', *, *, #751, .T. ) ;
#14783 = CARTESIAN_POINT ( 'NONE',  ( 0.000000000000000000, 0.09092130223458683158, -0.4724409448818898127 ) ) ;
#14784 = CARTESIAN_POINT ( 'NONE',  ( 0.05926487674657893168, 0.4498374011143063678, -1.934055118110236338 ) ) ;
#14786 = CIRCLE ( 'NONE', #12027, 0.5393700787401575214 ) ;
#14785 = CARTESIAN_POINT ( 'NONE',  ( 0.4585215200179055817, 0.03001016326913595253, -1.928289503579156516 ) ) ;
#14787 = VECTOR ( 'NONE', #3963, 39.37007874015748143 ) ;
#14788 = EDGE_CURVE ( 'NONE', #13649, #2754, #22274, .T. ) ;
#14789 = ORIENTED_EDGE ( 'NONE', *, *, #1906, .F. ) ;
#14790 = VERTEX_POINT ( 'NONE', #16705 ) ;
#14791 = CARTESIAN_POINT ( 'NONE',  ( -0.6068752646683485130, -0.1331980723927974342, -0.08786100608780256227 ) ) ;
#14792 = LINE ( 'NONE', #20695, #19467 ) ;
#14793 = DIRECTION ( 'NONE',  ( -1.000000000000000000, 0.000000000000000000, 0.000000000000000000 ) ) ;
#14794 = ORIENTED_EDGE ( 'NONE', *, *, #4995, .F. ) ;
#14795 = CARTESIAN_POINT ( 'NONE',  ( -0.1603262695921948977, -0.4410554214326551370, 0.07637549214372835182 ) ) ;
#14796 = CIRCLE ( 'NONE', #23790, 0.3464566929133857665 ) ;
#14797 = FACE_BOUND ( 'NONE', #20269, .T. ) ;
#14798 = CARTESIAN_POINT ( 'NONE',  ( 0.3858850602361924564, 0.2227473777836185831, -1.934055118110236116 ) ) ;
#14799 = ORIENTED_EDGE ( 'NONE', *, *, #18833, .F. ) ;
#14800 = CARTESIAN_POINT ( 'NONE',  ( 0.09187177619658809524, -0.3429980251342298336, 1.953740157480315043 ) ) ;
#14801 = EDGE_LOOP ( 'NONE', ( #10138, #13191, #22962, #26342 ) ) ;
#14802 = AXIS2_PLACEMENT_3D ( 'NONE', #1213, #11379, #22117 ) ;
#14803 = CARTESIAN_POINT ( 'NONE',  ( -0.5551587109978235457, -0.2272353400451556926, -0.2684417395417463270 ) ) ;
#14804 = CARTESIAN_POINT ( 'NONE',  ( 0.000000000000000000, 0.000000000000000000, -0.05856299212598425896 ) ) ;
#14805 = ORIENTED_EDGE ( 'NONE', *, *, #11442, .F. ) ;
#14806 = VERTEX_POINT ( 'NONE', #15024 ) ;
#14807 = CARTESIAN_POINT ( 'NONE',  ( -0.3355349563089153886, 0.1206850104808647739, -0.07874015748031495954 ) ) ;
#14808 = EDGE_CURVE ( 'NONE', #14790, #14897, #19132, .T. ) ;
#14809 = ADVANCED_FACE ( 'NONE', ( #25883 ), #4411, .F. ) ;
#14810 = CARTESIAN_POINT ( 'NONE',  ( 0.3349073414798194315, 0.1651192144506304638, -3.115157480314960647 ) ) ;
#14811 = LINE ( 'NONE', #23420, #24746 ) ;
#14812 = DIRECTION ( 'NONE',  ( -1.000000000000000000, 0.000000000000000000, 0.000000000000000000 ) ) ;
#14813 = CYLINDRICAL_SURFACE ( 'NONE', #4931, 0.1181102362204720091 ) ;
#14814 = AXIS2_PLACEMENT_3D ( 'NONE', #12302, #20925, #1569 ) ;
#14815 = LINE ( 'NONE', #23825, #3700 ) ;
#14816 = CARTESIAN_POINT ( 'NONE',  ( 0.1279527559055118058, 0.000000000000000000, 0.000000000000000000 ) ) ;
#14817 = AXIS2_PLACEMENT_3D ( 'NONE', #11094, #12657, #4052 ) ;
#14818 = ORIENTED_EDGE ( 'NONE', *, *, #12510, .F. ) ;
#14819 = CARTESIAN_POINT ( 'NONE',  ( 0.2530774914995135849, 0.5130713940405263740, 0.9399606299212600602 ) ) ;
#14820 = EDGE_LOOP ( 'NONE', ( #22242, #20673 ) ) ;
#14821 = DIRECTION ( 'NONE',  ( 0.000000000000000000, 1.000000000000000000, 0.000000000000000000 ) ) ;
#14822 = ( CONVERSION_BASED_UNIT ( 'INCH', #18876 ) LENGTH_UNIT ( ) NAMED_UNIT ( #27277 ) ) ;
#14823 = B_SPLINE_CURVE_WITH_KNOTS ( 'NONE', 3,
 ( #11723, #13848, #17795, #11309 ),
 .UNSPECIFIED., .F., .F.,
 ( 4, 4 ),
 ( 1.743059029969430185, 1.744705333033729877 ),
 .UNSPECIFIED. ) ;
#14824 = LINE ( 'NONE', #25536, #7996 ) ;
#14825 = CARTESIAN_POINT ( 'NONE',  ( -0.1649135259617106886, 0.4856708409200803378, 1.747047244094488194 ) ) ;
#14826 = VERTEX_POINT ( 'NONE', #25317 ) ;
#14827 = EDGE_CURVE ( 'NONE', #18714, #6657, #13017, .T. ) ;
#14828 = ORIENTED_EDGE ( 'NONE', *, *, #9051, .F. ) ;
#14829 = CARTESIAN_POINT ( 'NONE',  ( 0.09269288654273812045, -0.3460635936744816399, -3.115157480314960647 ) ) ;
#14830 = DIRECTION ( 'NONE',  ( 1.000000000000000000, 5.737213000000000442E-16, 0.000000000000000000 ) ) ;
#14831 = ( LENGTH_UNIT ( ) NAMED_UNIT ( * ) SI_UNIT ( $, .METRE. ) ) ;
#14832 = CARTESIAN_POINT ( 'NONE',  ( 0.3976891862754212137, 0.7181140751201181560, -0.6642661073933326943 ) ) ;
#14833 = AXIS2_PLACEMENT_3D ( 'NONE', #989, #9576, #13688 ) ;
#14834 = CARTESIAN_POINT ( 'NONE',  ( 0.02190250779246040100, 0.3346456692913385988, 1.973425196850393970 ) ) ;
#14835 = ORIENTED_EDGE ( 'NONE', *, *, #10547, .T. ) ;
#14836 = ORIENTED_EDGE ( 'NONE', *, *, #21698, .F. ) ;
#14837 = AXIS2_PLACEMENT_3D ( 'NONE', #26439, #1031, #5404 ) ;
#14838 = CONICAL_SURFACE ( 'NONE', #23827, 0.2952755905511805778, 0.2617993875000016457 ) ;
#14839 = EDGE_LOOP ( 'NONE', ( #7003, #22475, #21716, #10305, #1193, #21265 ) ) ;
#14840 = ORIENTED_EDGE ( 'NONE', *, *, #14373, .T. ) ;
#14841 = CARTESIAN_POINT ( 'NONE',  ( -0.1610509776512037416, -0.4407912692718771175, 0.07637795275590551769 ) ) ;
#14842 = B_SPLINE_CURVE_WITH_KNOTS ( 'NONE', 3,
 ( #27154, #3532, #1429, #10043 ),
 .UNSPECIFIED., .F., .F.,
 ( 4, 4 ),
 ( 0.3000437156586439613, 0.3015484798814578316 ),
 .UNSPECIFIED. ) ;
#14843 = CONTEXT_DEPENDENT_SHAPE_REPRESENTATION ( #10339, #9839 ) ;
#14844 = DIRECTION ( 'NONE',  ( 1.000000000000000000, 0.000000000000000000, 0.000000000000000000 ) ) ;
#14845 = CARTESIAN_POINT ( 'NONE',  ( -0.0005696707463066809363, 0.4606295689977896179, 0.1903859677778869663 ) ) ;
#14846 = AXIS2_PLACEMENT_3D ( 'NONE', #9895, #16263, #1418 ) ;
#14847 = VERTEX_POINT ( 'NONE', #6125 ) ;
#14848 = AXIS2_PLACEMENT_3D ( 'NONE', #5321, #11817, #9399 ) ;
#14849 = DIRECTION ( 'NONE',  ( 0.000000000000000000, -0.8660254037844384856, 0.5000000000000003331 ) ) ;
#14850 = DIRECTION ( 'NONE',  ( 1.000000000000000000, 1.000000000000000078E-15, 0.000000000000000000 ) ) ;
#14851 = CARTESIAN_POINT ( 'NONE',  ( -0.5427308778234085640, -0.4036295907641927472, 0.1714462237544466250 ) ) ;
#14852 = CARTESIAN_POINT ( 'NONE',  ( 0.3334645669291338987, -5.862181872992126152E-06, -1.869015748010449007 ) ) ;
#14853 = PLANE ( 'NONE',  #12589 ) ;
#14854 = CIRCLE ( 'NONE', #6264, 0.4848217985909654137 ) ;
#14855 = CARTESIAN_POINT ( 'NONE',  ( -0.6057854838206414572, 1.115659691807754372, 0.04720470158478681094 ) ) ;
#14856 = CARTESIAN_POINT ( 'NONE',  ( -0.6299212598425196763, 0.000000000000000000, -0.01377952755905511792 ) ) ;
#14857 = EDGE_CURVE ( 'NONE', #27329, #21174, #19587, .T. ) ;
#14858 = CARTESIAN_POINT ( 'NONE',  ( -0.6102362204724409711, -1.112204724409448842, 0.000000000000000000 ) ) ;
#14859 = EDGE_CURVE ( 'NONE', #23305, #13098, #20125, .T. ) ;
#14860 = CARTESIAN_POINT ( 'NONE',  ( -0.01030706208231672687, 0.1968503937007873850, -3.193897637795275912 ) ) ;
#14861 = CARTESIAN_POINT ( 'NONE',  ( 0.000000000000000000, 0.000000000000000000, -0.2618110236220472231 ) ) ;
#14862 = EDGE_LOOP ( 'NONE', ( #6116, #11767 ) ) ;
#14863 = AXIS2_PLACEMENT_3D ( 'NONE', #8823, #26061, #7122 ) ;
#14864 = EDGE_LOOP ( 'NONE', ( #19181, #4689 ) ) ;
#14865 = DIRECTION ( 'NONE',  ( 0.000000000000000000, 0.000000000000000000, -1.000000000000000000 ) ) ;
#14866 = EDGE_CURVE ( 'NONE', #14958, #17898, #4162, .T. ) ;
#14867 = ORIENTED_EDGE ( 'NONE', *, *, #4152, .T. ) ;
#14868 = ORIENTED_EDGE ( 'NONE', *, *, #7300, .T. ) ;
#14869 = CARTESIAN_POINT ( 'NONE',  ( 0.1287090038540879000, 4.133240157480319260E-16, -0.1968503937007877458 ) ) ;
#14870 = CARTESIAN_POINT ( 'NONE',  ( 0.4931450244001936989, 0.08715529520342342462, 0.09684793308443523374 ) ) ;
#14871 = EDGE_CURVE ( 'NONE', #19035, #17310, #24029, .T. ) ;
#14872 = EDGE_CURVE ( 'NONE', #1498, #26351, #9645, .T. ) ;
#14873 = FACE_OUTER_BOUND ( 'NONE', #25962, .T. ) ;
#14874 = CARTESIAN_POINT ( 'NONE',  ( 0.5335524835332355886, 0.1429116519061127411, 0.9202755905511811330 ) ) ;
#14875 = DIRECTION ( 'NONE',  ( 0.000000000000000000, 0.000000000000000000, -1.000000000000000000 ) ) ;
#14876 = ORIENTED_EDGE ( 'NONE', *, *, #24173, .T. ) ;
#14877 = DIRECTION ( 'NONE',  ( 0.000000000000000000, -1.000000000000000000, 0.000000000000000000 ) ) ;
#14878 = VECTOR ( 'NONE', #9990, 39.37007874015748143 ) ;
#14879 = AXIS2_PLACEMENT_3D ( 'NONE', #14816, #16917, #4056 ) ;
#14880 = CARTESIAN_POINT ( 'NONE',  ( -0.4563437504967154390, 0.07988585396358348356, 0.2048502514591916679 ) ) ;
#14881 = CARTESIAN_POINT ( 'NONE',  ( 0.000000000000000000, 0.000000000000000000, 0.2574803149606298969 ) ) ;
#14882 = APPLICATION_CONTEXT ( 'automotive_design' ) ;
#14883 = CARTESIAN_POINT ( 'NONE',  ( -0.04956879678459434613, 0.2165354330708661457, -3.634230943941107572 ) ) ;
#14884 = ORIENTED_EDGE ( 'NONE', *, *, #22420, .F. ) ;
#14885 = CARTESIAN_POINT ( 'NONE',  ( -0.1707210962531915677, -0.4707890492249701131, 0.09685039370078740717 ) ) ;
#14886 = DIRECTION ( 'NONE',  ( 0.000000000000000000, 0.000000000000000000, -1.000000000000000000 ) ) ;
#14887 = EDGE_LOOP ( 'NONE', ( #2606, #26193, #8035, #2335 ) ) ;
#14888 = FACE_OUTER_BOUND ( 'NONE', #1940, .T. ) ;
#14889 = CARTESIAN_POINT ( 'NONE',  ( -0.5131133041953912510, 0.2529800193559492705, 0.9399606299212598381 ) ) ;
#14890 = CARTESIAN_POINT ( 'NONE',  ( 0.1608692170993911430, -0.4408576787418653775, 0.07637630773773071424 ) ) ;
#14891 = VERTEX_POINT ( 'NONE', #2412 ) ;
#14892 = CARTESIAN_POINT ( 'NONE',  ( 0.3392634445559961631, 0.1151354519027797119, -3.115157480314959759 ) ) ;
#14893 = EDGE_CURVE ( 'NONE', #11904, #19560, #225, .T. ) ;
#14894 = CIRCLE ( 'NONE', #10338, 0.1003956692913385573 ) ;
#14895 = AXIS2_PLACEMENT_3D ( 'NONE', #4561, #8796, #17414 ) ;
#14896 = ADVANCED_FACE ( 'NONE', ( #19520 ), #25455, .F. ) ;
#14897 = VERTEX_POINT ( 'NONE', #11174 ) ;
#14898 = CARTESIAN_POINT ( 'NONE',  ( 0.3855916753034099864, -0.3382184156749167836, -1.550196850393700920 ) ) ;
#14899 = CARTESIAN_POINT ( 'NONE',  ( 0.5130713940404153517, -0.2530774915000200687, 0.9399606299212601712 ) ) ;
#14900 = ADVANCED_FACE ( 'NONE', ( #11311 ), #22744, .T. ) ;
#14901 = CARTESIAN_POINT ( 'NONE',  ( 0.4685039370078740717, 5.737518468446261360E-17, -6.283251968503937502E-17 ) ) ;
#14902 = CARTESIAN_POINT ( 'NONE',  ( -0.5811930530674194184, -0.4724394499398544278, -0.9954595798869386725 ) ) ;
#14903 = CARTESIAN_POINT ( 'NONE',  ( -0.0002221395201540506592, 0.5322834645669292097, 0.1322810039474933141 ) ) ;
#14904 = EDGE_LOOP ( 'NONE', ( #274, #22549, #17838, #512 ) ) ;
#14905 = CARTESIAN_POINT ( 'NONE',  ( -0.6299212598425196763, -0.6348133144914134274, -0.8891632684400255782 ) ) ;
#14906 = CARTESIAN_POINT ( 'NONE',  ( -0.2720459371704843088, 0.3242117229735834716, 0.2145688976377952695 ) ) ;
#14907 = CARTESIAN_POINT ( 'NONE',  ( 0.4068047116062469826, 0.4858504993706820874, 0.1061598535666330306 ) ) ;
#14908 = EDGE_CURVE ( 'NONE', #19722, #19742, #5612, .T. ) ;
#14909 = CARTESIAN_POINT ( 'NONE',  ( 0.01504182353227358389, -0.2012500529900838608, 2.464602332225414408E-17 ) ) ;
#14910 = CIRCLE ( 'NONE', #24787, 0.3937007874015748254 ) ;
#14911 = ADVANCED_FACE ( 'NONE', ( #22185 ), #11015, .F. ) ;
#14912 = VECTOR ( 'NONE', #15490, 39.37007874015748143 ) ;
#14913 = DIRECTION ( 'NONE',  ( 1.000000000000000000, 0.000000000000000000, 0.000000000000000000 ) ) ;
#14914 = ORIENTED_EDGE ( 'NONE', *, *, #86, .F. ) ;
#14915 = CARTESIAN_POINT ( 'NONE',  ( 0.000000000000000000, 0.1751968503937007815, 0.000000000000000000 ) ) ;
#14916 = CARTESIAN_POINT ( 'NONE',  ( -0.4889536969035310210, -0.06441834428467370366, -1.569881889763779625 ) ) ;
#14917 = B_SPLINE_CURVE_WITH_KNOTS ( 'NONE', 3,
 ( #10117, #12239, #12380, #4053 ),
 .UNSPECIFIED., .F., .F.,
 ( 4, 4 ),
 ( 1.006307675027575899, 1.007953978091874037 ),
 .UNSPECIFIED. ) ;
#14918 = CARTESIAN_POINT ( 'NONE',  ( -0.05926487674658171417, -0.4498374011143209117, -1.934055118110236338 ) ) ;
#14919 = CIRCLE ( 'NONE', #4955, 0.3937007874015748254 ) ;
#14920 = EDGE_CURVE ( 'NONE', #25917, #12651, #13269, .T. ) ;
#14921 = EDGE_LOOP ( 'NONE', ( #14324, #20067, #16162, #5671 ) ) ;
#14922 = CARTESIAN_POINT ( 'NONE',  ( -0.5355664161054535244, -0.2721702372959802774, -0.2828063903444661409 ) ) ;
#14923 = CARTESIAN_POINT ( 'NONE',  ( 0.000000000000000000, 0.000000000000000000, 0.02362204724409448786 ) ) ;
#14924 = EDGE_CURVE ( 'NONE', #26747, #22411, #6948, .T. ) ;
#14925 = CARTESIAN_POINT ( 'NONE',  ( 0.6614173228346456046, 8.100026073100603114E-17, -0.2480314960629921295 ) ) ;
#14926 = ORIENTED_EDGE ( 'NONE', *, *, #25777, .F. ) ;
#14927 = AXIS2_PLACEMENT_3D ( 'NONE', #1819, #5791, #10145 ) ;
#14928 = DIRECTION ( 'NONE',  ( 0.000000000000000000, 0.000000000000000000, -1.000000000000000000 ) ) ;
#14929 = CARTESIAN_POINT ( 'NONE',  ( 9.642888182262624280E-17, 0.9055118110236221041, 0.7874015748031496509 ) ) ;
#14930 = CARTESIAN_POINT ( 'NONE',  ( 0.000000000000000000, 0.000000000000000000, 0.1377952755905511584 ) ) ;
#14931 = CARTESIAN_POINT ( 'NONE',  ( -0.4219236230595549419, 0.1431838228107190636, -1.934055118110236116 ) ) ;
#14932 = EDGE_CURVE ( 'NONE', #8592, #9665, #24302, .T. ) ;
#14933 = VERTEX_POINT ( 'NONE', #21778 ) ;
#14934 = CARTESIAN_POINT ( 'NONE',  ( 0.2669480828848183052, -0.2341512108694381034, 1.953740157480315043 ) ) ;
#14935 = VERTEX_POINT ( 'NONE', #19930 ) ;
#14936 = CIRCLE ( 'NONE', #5436, 0.4803149606299212393 ) ;
#14937 = CARTESIAN_POINT ( 'NONE',  ( -0.5298607097989774806, -0.2854075319011052381, -0.2877231093509545201 ) ) ;
#14938 = CARTESIAN_POINT ( 'NONE',  ( 0.000000000000000000, 0.000000000000000000, -0.006889763779527558960 ) ) ;
#14939 = CARTESIAN_POINT ( 'NONE',  ( -1.466875984251968630E-17, 0.000000000000000000, -0.02362204724409448786 ) ) ;
#14940 = DIRECTION ( 'NONE',  ( 0.000000000000000000, 0.000000000000000000, -1.000000000000000000 ) ) ;
#14941 = EDGE_CURVE ( 'NONE', #3411, #25669, #18202, .T. ) ;
#14942 = CARTESIAN_POINT ( 'NONE',  ( -0.1867299569291481776, 0.3233561589688985771, -3.115157480314960647 ) ) ;
#14943 = CARTESIAN_POINT ( 'NONE',  ( 0.4930758245789425009, 0.08754571829529310401, 0.2574803149606298969 ) ) ;
#14944 = FACE_OUTER_BOUND ( 'NONE', #8798, .T. ) ;
#14945 = DIRECTION ( 'NONE',  ( -1.000000000000000000, 0.000000000000000000, 0.000000000000000000 ) ) ;
#14946 = CARTESIAN_POINT ( 'NONE',  ( -0.1771653543307086520, 1.482715313533957208E-17, 0.1673228346456692994 ) ) ;
#14947 = AXIS2_PLACEMENT_3D ( 'NONE', #5464, #20992, #14667 ) ;
#14948 = CARTESIAN_POINT ( 'NONE',  ( -0.6996455634166303117, -0.1588938903163411021, 0.3122824329290380674 ) ) ;
#14949 = CARTESIAN_POINT ( 'NONE',  ( -0.3642352168757148068, 0.4152525734086684461, 0.9202755905511811330 ) ) ;
#14950 = ORIENTED_EDGE ( 'NONE', *, *, #969, .F. ) ;
#14951 = CARTESIAN_POINT ( 'NONE',  ( 0.3713448905834433322, 0.06600512665679410251, 0.1992125984251968684 ) ) ;
#14952 = ADVANCED_FACE ( 'NONE', ( #7208, #23910 ), #2547, .T. ) ;
#14953 = EDGE_LOOP ( 'NONE', ( #15504, #8977, #9951, #19145 ) ) ;
#14954 = ORIENTED_EDGE ( 'NONE', *, *, #3378, .T. ) ;
#14955 = DIRECTION ( 'NONE',  ( 0.000000000000000000, -1.000000000000000000, 0.000000000000000000 ) ) ;
#14956 = CARTESIAN_POINT ( 'NONE',  ( -0.5118110236220472231, 0.03349795313264340019, 1.766732283464566899 ) ) ;
#14957 = EDGE_CURVE ( 'NONE', #26680, #26488, #3435, .T. ) ;
#14958 = VERTEX_POINT ( 'NONE', #15440 ) ;
#14959 = ORIENTED_EDGE ( 'NONE', *, *, #27786, .T. ) ;
#14961 = CARTESIAN_POINT ( 'NONE',  ( 0.1151913129404385921, 0.3392387706403768299, -3.115157480314960647 ) ) ;
#14960 = CARTESIAN_POINT ( 'NONE',  ( -0.6512499169102675678, 0.1155267097730827697, 0.1926811207693707451 ) ) ;
#14962 = VERTEX_POINT ( 'NONE', #17662 ) ;
#14963 = DIRECTION ( 'NONE',  ( 0.000000000000000000, 1.000000000000000000, 0.000000000000000000 ) ) ;
#14964 = CARTESIAN_POINT ( 'NONE',  ( 0.3976891862754212137, 0.8566358266442657410, -0.5893543329197449276 ) ) ;
#14965 = B_SPLINE_CURVE_WITH_KNOTS ( 'NONE', 3,
 ( #23782, #4280, #21931, #462, #26027, #4551, #12747, #19801 ),
 .UNSPECIFIED., .F., .F.,
 ( 4, 2, 2, 4 ),
 ( 0.000000000000000000, 0.1249999999999999445, 0.2500000000000000555, 0.5000000000000000000 ),
 .UNSPECIFIED. ) ;
#14966 = CARTESIAN_POINT ( 'NONE',  ( 0.3346456692913385988, -0.02190250779246876237, 1.973425196850393970 ) ) ;
#14967 = ORIENTED_EDGE ( 'NONE', *, *, #27695, .F. ) ;
#14968 = ORIENTED_EDGE ( 'NONE', *, *, #8901, .F. ) ;
#14969 = CIRCLE ( 'NONE', #26640, 0.5322834645669292097 ) ;
#14970 = CARTESIAN_POINT ( 'NONE',  ( 0.4763861460130704994, -0.1275996891957771051, -1.550196850393700920 ) ) ;
#14971 = FACE_BOUND ( 'NONE', #11785, .T. ) ;
#14972 = VERTEX_POINT ( 'NONE', #13423 ) ;
#14973 = ORIENTED_EDGE ( 'NONE', *, *, #12274, .F. ) ;
#14974 = ORIENTED_EDGE ( 'NONE', *, *, #13633, .F. ) ;
#14975 = CARTESIAN_POINT ( 'NONE',  ( 0.000000000000000000, 0.000000000000000000, -3.278217716535432842E-17 ) ) ;
#14976 = AXIS2_PLACEMENT_3D ( 'NONE', #2533, #4254, #11156 ) ;
#14977 = DIRECTION ( 'NONE',  ( -1.000000000000000000, 0.000000000000000000, 0.000000000000000000 ) ) ;
#14978 = B_SPLINE_CURVE_WITH_KNOTS ( 'NONE', 3,
 ( #23375, #12619, #8386, #16565, #23226, #5850, #14473, #12476, #1596, #10200, #1738, #18818, #27455, #16716, #25475, #10349, #18965 ),
 .UNSPECIFIED., .F., .F.,
 ( 4, 2, 2, 1, 2, 2, 2, 2, 4 ),
 ( 0.08984410253495091203, 0.2036135897180814669, 0.2604983333096470011, 0.3173830769012125352, 0.4311525640843440477, 0.5449220512674757266, 0.6586915384506072391, 0.7724610256337387515, 1.000000000000000000 ),
 .UNSPECIFIED. ) ;
#14979 = CARTESIAN_POINT ( 'NONE',  ( -0.03532354024591893848, -1.576771653543307172, 9.184850993605150903E-17 ) ) ;
#14980 = CARTESIAN_POINT ( 'NONE',  ( 0.4216473063920845865, -0.2427620699802750248, 0.2467937632982898366 ) ) ;
#14981 = ORIENTED_EDGE ( 'NONE', *, *, #4333, .T. ) ;
#14982 = CARTESIAN_POINT ( 'NONE',  ( -0.6709908451338799651, -0.1528902114222696895, 0.1322810039474933141 ) ) ;
#14983 = CARTESIAN_POINT ( 'NONE',  ( 0.6881889763779527325, 0.000000000000000000, 0.1322834645669291320 ) ) ;
#14984 = DIRECTION ( 'NONE',  ( -0.7071067811865480168, 0.7071067811865470176, 0.000000000000000000 ) ) ;
#14985 = CIRCLE ( 'NONE', #10890, 0.1003956692913385851 ) ;
#14986 = SPHERICAL_SURFACE ( 'NONE', #21182, 0.1299232283464566984 ) ;
#14987 = CARTESIAN_POINT ( 'NONE',  ( -0.6204317524930640371, 1.098416878719267187, 0.09031125883760274253 ) ) ;
#14988 = FACE_OUTER_BOUND ( 'NONE', #1224, .T. ) ;
#14989 = CARTESIAN_POINT ( 'NONE',  ( -0.5314960629921260393, 6.402768735150616610E-17, 1.747047244094488194 ) ) ;
#14990 = EDGE_CURVE ( 'NONE', #9428, #7703, #26284, .T. ) ;
#14991 = CYLINDRICAL_SURFACE ( 'NONE', #25219, 0.3346456692913385988 ) ;
#14992 = B_SPLINE_CURVE_WITH_KNOTS ( 'NONE', 3,
 ( #24331, #2575, #11200, #9074, #17688, #20094, #7236, #26313, #15852, #13878 ),
 .UNSPECIFIED., .F., .F.,
 ( 4, 2, 2, 2, 4 ),
 ( 0.000000000000000000, 0.2500000000000001665, 0.5000000000000003331, 0.7500000000000001110, 1.000000000000000000 ),
 .UNSPECIFIED. ) ;
#14993 = CARTESIAN_POINT ( 'NONE',  ( 0.01288382760289561585, 0.2165354330708661457, -3.174212598425197207 ) ) ;
#14994 = ORIENTED_EDGE ( 'NONE', *, *, #19595, .T. ) ;
#14995 = CARTESIAN_POINT ( 'NONE',  ( 0.3119936278817372344, -0.6460736482317533946, 0.1601585119437425875 ) ) ;
#14996 = ( LENGTH_UNIT ( ) NAMED_UNIT ( * ) SI_UNIT ( $, .METRE. ) ) ;
#14997 = ORIENTED_EDGE ( 'NONE', *, *, #17288, .F. ) ;
#14998 = FACE_OUTER_BOUND ( 'NONE', #26073, .T. ) ;
#14999 = CARTESIAN_POINT ( 'NONE',  ( -0.3759206409296169671, 0.2989751379763689321, 0.2194422276316772835 ) ) ;
#15000 = CARTESIAN_POINT ( 'NONE',  ( 0.3528204557977369094, 0.06272520244126274236, 0.1805249803451361157 ) ) ;
#15001 = ORIENTED_EDGE ( 'NONE', *, *, #27438, .T. ) ;
#15002 = CARTESIAN_POINT ( 'NONE',  ( 0.2315507648392299000, -0.4792806379917101678, 0.3401574803149606252 ) ) ;
#15003 = DIRECTION ( 'NONE',  ( 1.000000000000000000, 0.000000000000000000, 0.000000000000000000 ) ) ;
#15004 = CIRCLE ( 'NONE', #10458, 0.05216535433070866590 ) ;
#15005 = CARTESIAN_POINT ( 'NONE',  ( 0.3214446924536846772, 0.3840069416942866742, 0.2574803149606298969 ) ) ;
#15006 = CARTESIAN_POINT ( 'NONE',  ( 0.000000000000000000, 0.3937007874015748254, 0.02362204724409448786 ) ) ;
#15007 = CARTESIAN_POINT ( 'NONE',  ( -0.8725268807032540153, 0.000000000000000000, -1.052618110236220428 ) ) ;
#15008 = SHAPE_REPRESENTATION ( 'Deep Groove Ball Bearing 20x42x12', ( #11588 ), #1261 ) ;
#15009 = ADVANCED_FACE ( 'NONE', ( #5806 ), #2954, .F. ) ;
#15010 = CIRCLE ( 'NONE', #16812, 0.6889763779527560139 ) ;
#15011 = ORIENTED_EDGE ( 'NONE', *, *, #20889, .T. ) ;
#15012 = CARTESIAN_POINT ( 'NONE',  ( 0.1658556822975960354, -0.4573967274768249713, 0.1075369453260532765 ) ) ;
#15013 = CARTESIAN_POINT ( 'NONE',  ( -5.747161356628524594E-17, -0.4692913385826771866, -3.278217716535432842E-17 ) ) ;
#15014 = CARTESIAN_POINT ( 'NONE',  ( 0.000000000000000000, 4.580371886574746102E-17, 0.3740157480314960647 ) ) ;
#15015 = CIRCLE ( 'NONE', #11371, 0.07677362204724412498 ) ;
#15016 = CARTESIAN_POINT ( 'NONE',  ( -0.4986013261500205074, 0.000000000000000000, -0.1309055118110236116 ) ) ;
#15017 = CARTESIAN_POINT ( 'NONE',  ( 0.003937007874015826907, -0.09842519685039370636, 1.205361022782828035E-17 ) ) ;
#15018 = CARTESIAN_POINT ( 'NONE',  ( 0.5230301363771271417, 0.1775991818008589573, 0.9399606299212598381 ) ) ;
#15019 = PLANE ( 'NONE',  #20708 ) ;
#15020 = ADVANCED_FACE ( 'NONE', ( #7780 ), #18342, .F. ) ;
#15021 = DIRECTION ( 'NONE',  ( 0.000000000000000000, 0.000000000000000000, 1.000000000000000000 ) ) ;
#15022 = ORIENTED_EDGE ( 'NONE', *, *, #8155, .F. ) ;
#15023 = B_SPLINE_SURFACE_WITH_KNOTS ( 'NONE', 2, 3, ( 
 ( #26074, #13351, #21975, #22243, #15368, #15628, #784, #9371, #17976, #26612, #15887, #24490, #13766, #11644, #23959, #14056, #18550, #20687, #16588, #20822, #27330, #22812, #25061, #5728, #7846, #14342, #9666, #3159, #24630, #18263, #1341, #16317, #3433, #22956, #12070, #23098, #27053, #14492, #7981, #1070, #16450, #18110, #3572, #9946, #12350, #3727, #5579, #20970, #24920, #27196, #12207, #1473, #10085, #11786, #14205, #18693, #20405, #26902, #25201, #5868, #3294, #9510, #22668, #26759, #7409, #16032 ),
 ( #11934, #7552, #5288, #16179, #20552, #13913, #22531, #24779, #7704, #5443, #1207, #9807, #18407, #17153, #18831, #15052, #4158, #21531, #14784, #23389, #13047, #23525, #16727, #12631, #25340, #4440, #12768, #8668, #6283, #10503, #6559, #21393, #15183, #12495, #17287, #23797, #1613, #8532, #23666, #17020, #19408, #2032, #23244, #25769, #4299, #101, #6005, #25628, #21109, #27473, #14918, #14642, #25910, #10644, #10217, #8121, #8399, #6418, #1751, #3876, #10364, #27759, #19264, #18983, #21508, #12903 ),
 ( #2173, #1892, #19121, #27614, #16885, #8256, #10789, #25492, #6157, #4020, #21253, #5101, #15849, #13173, #9071, #6695, #4831, #6973, #24450, #13587, #15336, #17419, #4973, #26571, #19692, #22208, #26178, #8938, #17684, #21947, #13447, #10927, #7230, #21804, #22070, #19954, #21669, #2441, #17567, #2701, #2299, #11068, #15720, #23931, #26436, #4566, #26042, #2836, #606, #6831, #15596, #15461, #11336, #9200, #743, #11472, #20089, #24196, #17819, #7103, #24324, #9333, #361, #24057, #8804, #4692 ) ),
 .UNSPECIFIED., .F., .T., .F.,
 ( 3, 3 ),
 ( 4, 2, 2, 2, 2, 2, 2, 2, 2, 2, 2, 2, 2, 2, 2, 2, 2, 2, 2, 2, 2, 2, 2, 2, 2, 2, 2, 2, 2, 2, 2, 2, 4 ),
 ( 0.000000000000000000, 1.000000000000000000 ),
 ( 0.000000000000000000, 0.1963495408493620697, 0.3926990816987241395, 0.5890486225480862092, 0.7853981633974482790, 0.9817477042468103487, 1.178097245096172418, 1.374446785945534488, 1.570796326794896558, 1.767145867644258628, 1.963495408493620697, 2.159844949342982545, 2.356194490192344837, 2.552544031041707129, 2.748893571891068976, 2.945243112740430824, 3.141592653589793116, 3.337942194439155408, 3.534291735288517255, 3.730641276137879103, 3.926990816987241395, 4.123340357836603687, 4.319689898685965090, 4.516039439535327382, 4.712388980384689674, 4.908738521234051966, 5.105088062083414258, 5.301437602932775661, 5.497787143782137953, 5.694136684631500245, 5.890486225480861648, 6.086835766330223940, 6.283185307179586232 ),
 .UNSPECIFIED. ) ;
#15024 = CARTESIAN_POINT ( 'NONE',  ( -0.03532354024591901481, -0.8267716535433071723, -0.8267716535433070613 ) ) ;
#15025 = AXIS2_PLACEMENT_3D ( 'NONE', #4743, #15511, #24242 ) ;
#15026 = CIRCLE ( 'NONE', #19524, 0.1181102362204720091 ) ;
#15027 = ORIENTED_EDGE ( 'NONE', *, *, #15197, .F. ) ;
#15028 = AXIS2_PLACEMENT_3D ( 'NONE', #25737, #10181, #19232 ) ;
#15029 = CARTESIAN_POINT ( 'NONE',  ( -0.4441657790094368230, 0.2564944395535841970, -1.550196850393700920 ) ) ;
#15030 = CARTESIAN_POINT ( 'NONE',  ( -0.5672055940112499250, -0.07462095020172467008, 0.9399606299212600602 ) ) ;
#15031 = FACE_OUTER_BOUND ( 'NONE', #18070, .T. ) ;
#15032 = DIRECTION ( 'NONE',  ( 0.000000000000000000, -1.000000000000000000, 0.000000000000000000 ) ) ;
#15033 = CARTESIAN_POINT ( 'NONE',  ( -0.5280904602948607307, -0.06947618719658474329, 1.747047244094487972 ) ) ;
#15034 = CARTESIAN_POINT ( 'NONE',  ( -0.2307318466671160750, 0.2741888764709654036, 0.1805249803371026529 ) ) ;
#15035 = ORIENTED_EDGE ( 'NONE', *, *, #21568, .T. ) ;
#15036 = CARTESIAN_POINT ( 'NONE',  ( -0.1361267291514174083, -0.1666946003182495917, -0.2490847877778887554 ) ) ;
#15037 = CARTESIAN_POINT ( 'NONE',  ( -0.4932821129636645874, 0.08637579872942342807, 0.09685039370078740717 ) ) ;
#15038 = CARTESIAN_POINT ( 'NONE',  ( -0.3995066426835598983, 0.4757712504659716291, 0.2574827755769819038 ) ) ;
#15039 = ORIENTED_EDGE ( 'NONE', *, *, #9851, .T. ) ;
#15040 = AXIS2_PLACEMENT_3D ( 'NONE', #16429, #18246, #20806 ) ;
#15041 = DIRECTION ( 'NONE',  ( 0.000000000000000000, 7.180547322999998243E-06, -0.9999999999742198442 ) ) ;
#15042 = EDGE_CURVE ( 'NONE', #16233, #6811, #26987, .T. ) ;
#15043 = CONICAL_SURFACE ( 'NONE', #20417, 0.4092416079569000109, 0.7340599135827593491 ) ;
#15044 = DIRECTION ( 'NONE',  ( 0.000000000000000000, 0.000000000000000000, -1.000000000000000000 ) ) ;
#15045 = ORIENTED_EDGE ( 'NONE', *, *, #3875, .T. ) ;
#15046 = EDGE_CURVE ( 'NONE', #14659, #17723, #3349, .T. ) ;
#15047 = LINE ( 'NONE', #6153, #21589 ) ;
#15048 = AXIS2_PLACEMENT_3D ( 'NONE', #9242, #20003, #2492 ) ;
#15049 = CARTESIAN_POINT ( 'NONE',  ( -0.1585706980422388890, 0.4669911931914605963, -1.550196850393700920 ) ) ;
#15050 = ADVANCED_FACE ( 'NONE', ( #20349 ), #22605, .F. ) ;
#15052 = CARTESIAN_POINT ( 'NONE',  ( -0.05926487674658593302, 0.4498374011143062567, -1.934055118110236338 ) ) ;
#15053 = ADVANCED_FACE ( 'NONE', ( #5376 ), #26840, .T. ) ;
#15054 = CARTESIAN_POINT ( 'NONE',  ( -0.4173228346456693272, 5.110730736599190647E-17, 0.4724409448818898127 ) ) ;
#15055 = ORIENTED_EDGE ( 'NONE', *, *, #27121, .F. ) ;
#15056 = ADVANCED_FACE ( 'NONE', ( #20629 ), #13292, .F. ) ;
#15057 = CARTESIAN_POINT ( 'NONE',  ( -0.5632721120450597807, -0.2087920062485354444, -0.2632549038600744407 ) ) ;
#15058 = DIRECTION ( 'NONE',  ( 1.000000000000000000, 0.000000000000000000, 0.000000000000000000 ) ) ;
#15059 = CARTESIAN_POINT ( 'NONE',  ( 0.0006345105826664493992, 0.4803145415259079121, 0.2362204724409449896 ) ) ;
#15060 = CARTESIAN_POINT ( 'NONE',  ( -0.03532354024591901481, -0.8267716535433071723, 0.000000000000000000 ) ) ;
#15061 = AXIS2_PLACEMENT_3D ( 'NONE', #21932, #19802, #17671 ) ;
#15062 = ORIENTED_EDGE ( 'NONE', *, *, #15544, .F. ) ;
#15063 = CIRCLE ( 'NONE', #18149, 0.3070866141732283561 ) ;
#15064 = DIRECTION ( 'NONE',  ( 1.000000000000000000, 0.000000000000000000, 0.000000000000000000 ) ) ;
#15065 = DIRECTION ( 'NONE',  ( 0.000000000000000000, 1.000000000000000000, 0.000000000000000000 ) ) ;
#15066 = AXIS2_PLACEMENT_3D ( 'NONE', #25956, #21854, #19455 ) ;
#15067 = CARTESIAN_POINT ( 'NONE',  ( 0.4219262446671240840, 0.1431849087161535528, -1.934055118110236560 ) ) ;
#15068 = CARTESIAN_POINT ( 'NONE',  ( -0.7121770198535963825, 0.2056174084053519757, 0.2200249214779901596 ) ) ;
#15069 = VERTEX_POINT ( 'NONE', #1145 ) ;
#15070 = VECTOR ( 'NONE', #14424, 39.37007874015748143 ) ;
#15071 = CARTESIAN_POINT ( 'NONE',  ( -0.5317387256069298074, -0.2810540235075434379, -0.2861221005886522284 ) ) ;
#15072 = VECTOR ( 'NONE', #26110, 39.37007874015748854 ) ;
#15073 = ( REPRESENTATION_RELATIONSHIP ('NONE','NONE', #12434, #4612 ) REPRESENTATION_RELATIONSHIP_WITH_TRANSFORMATION ( #8265 )SHAPE_REPRESENTATION_RELATIONSHIP( ) ) ;
#15074 = CARTESIAN_POINT ( 'NONE',  ( -0.3355349563089153886, 0.1011697176171429124, -0.2362204724409449064 ) ) ;
#15075 = EDGE_CURVE ( 'NONE', #17187, #11528, #27266, .T. ) ;
#15076 = CARTESIAN_POINT ( 'NONE',  ( 0.3726024258163779246, 0.02438677169350801990, -3.115157480314960647 ) ) ;
#15077 = CARTESIAN_POINT ( 'NONE',  ( 0.000000000000000000, 0.000000000000000000, 0.4488188976377953110 ) ) ;
#15078 = CARTESIAN_POINT ( 'NONE',  ( 1.692913385826771533, 0.07874015748031495954, 0.1181102362204723144 ) ) ;
#15079 = CARTESIAN_POINT ( 'NONE',  ( 2.632951206231566310, -0.4724409448818898127, -0.8182917201112815953 ) ) ;
#15080 = FACE_OUTER_BOUND ( 'NONE', #14432, .T. ) ;
#15081 = EDGE_CURVE ( 'NONE', #16432, #9819, #9211, .T. ) ;
#15082 = AXIS2_PLACEMENT_3D ( 'NONE', #8703, #17943, #11476 ) ;
#15083 = CARTESIAN_POINT ( 'NONE',  ( 1.857656692913385893E-16, 0.000000000000000000, 0.5118110235513823048 ) ) ;
#15084 = ORIENTED_EDGE ( 'NONE', *, *, #588, .T. ) ;
#15085 = CARTESIAN_POINT ( 'NONE',  ( 0.000000000000000000, 0.000000000000000000, -3.278217716535432842E-17 ) ) ;
#15086 = AXIS2_PLACEMENT_3D ( 'NONE', #3692, #3543, #12172 ) ;
#15087 = ORIENTED_EDGE ( 'NONE', *, *, #23719, .F. ) ;
#15088 = B_SPLINE_CURVE_WITH_KNOTS ( 'NONE', 3,
 ( #18392, #14191, #20110, #3142, #5127, #22232, #18250, #768 ),
 .UNSPECIFIED., .F., .F.,
 ( 4, 2, 2, 4 ),
 ( 0.5000000000000000000, 0.7499999999999996669, 0.8749999999999997780, 1.000000000000000000 ),
 .UNSPECIFIED. ) ;
#15089 = CIRCLE ( 'NONE', #15974, 0.4010740433761567081 ) ;
#15090 = DIRECTION ( 'NONE',  ( -1.000000000000000000, 0.000000000000000000, -0.000000000000000000 ) ) ;
#15091 = CYLINDRICAL_SURFACE ( 'NONE', #9049, 0.6881889763779527325 ) ;
#15092 = PRODUCT_CONTEXT ( 'NONE', #17041, 'mechanical' ) ;
#15093 = CARTESIAN_POINT ( 'NONE',  ( -0.1327036767659643679, -0.4954415918530851726, 1.766732283464566899 ) ) ;
#15094 = DIRECTION ( 'NONE',  ( 0.000000000000000000, 1.000000000000000000, 0.000000000000000000 ) ) ;
#15095 = EDGE_LOOP ( 'NONE', ( #11121, #22407, #27766, #10281, #793, #22438 ) ) ;
#15096 = VERTEX_POINT ( 'NONE', #7489 ) ;
#15098 = CARTESIAN_POINT ( 'NONE',  ( -0.1151913129404409791, -0.3392387706403589553, -3.115157480314960647 ) ) ;
#15097 = CARTESIAN_POINT ( 'NONE',  ( -0.6117062799105453808, 0.1085321106658580781, 0.09685039370078740717 ) ) ;
#15099 = ORIENTED_EDGE ( 'NONE', *, *, #9420, .F. ) ;
#15100 = ORIENTED_EDGE ( 'NONE', *, *, #5118, .T. ) ;
#15101 = CARTESIAN_POINT ( 'NONE',  ( 0.3102399269716953345, -0.7316071111737637578, -0.6652804359117283628 ) ) ;
#15102 = LENGTH_MEASURE_WITH_UNIT ( LENGTH_MEASURE( 0.02539999999999999897 ), #3784 ) ;
#15103 = DIRECTION ( 'NONE',  ( 1.000000000000000000, 0.000000000000000000, 0.000000000000000000 ) ) ;
#15104 = CIRCLE ( 'NONE', #14645, 0.4941010236220472751 ) ;
#15105 = CARTESIAN_POINT ( 'NONE',  ( -0.02190250779245987017, -0.3346456692913387099, 1.973425196850393970 ) ) ;
#15106 = ORIENTED_EDGE ( 'NONE', *, *, #3329, .T. ) ;
#15107 = ORIENTED_EDGE ( 'NONE', *, *, #27146, .T. ) ;
#15108 = CARTESIAN_POINT ( 'NONE',  ( 0.6118978891064172920, 0.1074467966294246069, 0.09684874924366436433 ) ) ;
#15109 = ORIENTED_EDGE ( 'NONE', *, *, #8618, .F. ) ;
#15110 = ORIENTED_EDGE ( 'NONE', *, *, #3666, .F. ) ;
#15111 = ORIENTED_EDGE ( 'NONE', *, *, #1876, .F. ) ;
#15112 = B_SPLINE_CURVE_WITH_KNOTS ( 'NONE', 3,
 ( #17192, #17465, #25808, #6456, #23837, #23702 ),
 .UNSPECIFIED., .F., .F.,
 ( 4, 2, 4 ),
 ( 0.000000000000000000, 0.2500000000000000000, 0.5000000000000000000 ),
 .UNSPECIFIED. ) ;
#15114 = EDGE_CURVE ( 'NONE', #16237, #20499, #6525, .T. ) ;
#15113 = AXIS2_PLACEMENT_3D ( 'NONE', #9144, #17763, #11410 ) ;
#15115 = CARTESIAN_POINT ( 'NONE',  ( 0.01230314960629921330, 0.000000000000000000, 0.000000000000000000 ) ) ;
#15116 = CIRCLE ( 'NONE', #12833, 0.3740157480314960647 ) ;
#15117 = CARTESIAN_POINT ( 'NONE',  ( -0.09334068553655658351, 0.3008231328410254091, -3.580124219708414657 ) ) ;
#15118 = B_SPLINE_CURVE_WITH_KNOTS ( 'NONE', 3,
 ( #11234, #8840, #7009, #26347, #4477, #15765, #17464, #269 ),
 .UNSPECIFIED., .F., .F.,
 ( 4, 2, 2, 4 ),
 ( 0.000000000000000000, 0.1249999999999999722, 0.2499999999999999445, 0.5000000000000000000 ),
 .UNSPECIFIED. ) ;
#15119 = FACE_OUTER_BOUND ( 'NONE', #4896, .T. ) ;
#15120 = EDGE_LOOP ( 'NONE', ( #13903, #17075, #27670, #10009, #4760 ) ) ;
#15121 = EDGE_CURVE ( 'NONE', #15981, #14114, #16270, .T. ) ;
#15122 = CARTESIAN_POINT ( 'NONE',  ( 0.3268939675028499914, -0.1881330340946397728, 0.1992125984251968684 ) ) ;
#15123 = AXIS2_PLACEMENT_3D ( 'NONE', #15533, #15406, #17884 ) ;
#15124 = CARTESIAN_POINT ( 'NONE',  ( -0.5648342936079289167, 1.117528104686835722, 0.04027680511158680116 ) ) ;
#15125 = DIRECTION ( 'NONE',  ( -0.4338837391175582869, -0.9009688679024190350, 0.000000000000000000 ) ) ;
#15126 = DIRECTION ( 'NONE',  ( 0.000000000000000000, 0.000000000000000000, 1.000000000000000000 ) ) ;
#15127 = DIRECTION ( 'NONE',  ( 0.000000000000000000, 1.000000000000000000, 0.000000000000000000 ) ) ;
#15128 = EDGE_CURVE ( 'NONE', #14684, #6454, #22759, .T. ) ;
#15129 = AXIS2_PLACEMENT_3D ( 'NONE', #4770, #2371, #11004 ) ;
#15130 = CARTESIAN_POINT ( 'NONE',  ( 0.1516263115863346334, 0.1971492568089275588, 0.4530651079966787620 ) ) ;
#15131 = VERTEX_POINT ( 'NONE', #27264 ) ;
#15132 = CIRCLE ( 'NONE', #21871, 1.131889763779527547 ) ;
#15133 = CARTESIAN_POINT ( 'NONE',  ( 0.1634143070183528834, -0.4472844159282008958, 0.2330651858545649824 ) ) ;
#15134 = VERTEX_POINT ( 'NONE', #7919 ) ;
#15135 = CARTESIAN_POINT ( 'NONE',  ( -0.1718374205099799101, -0.4703827404237102550, 0.09685039370078740717 ) ) ;
#15136 = CARTESIAN_POINT ( 'NONE',  ( -0.5610237960480470853, 1.122047070076019448, -0.01921884795634628412 ) ) ;
#15137 = FACE_OUTER_BOUND ( 'NONE', #24374, .T. ) ;
#15138 = ORIENTED_EDGE ( 'NONE', *, *, #13446, .F. ) ;
#15139 = CARTESIAN_POINT ( 'NONE',  ( 0.2762247810519017355, -0.4783323773986510319, 0.9202755905511811330 ) ) ;
#15140 = CIRCLE ( 'NONE', #7908, 0.1181010187939084827 ) ;
#15141 = CARTESIAN_POINT ( 'NONE',  ( 0.3882259019058474370, 0.3087756353523146702, 0.2989974301447032579 ) ) ;
#15142 = ORIENTED_EDGE ( 'NONE', *, *, #7364, .F. ) ;
#15143 = DIRECTION ( 'NONE',  ( 0.000000000000000000, 0.000000000000000000, -1.000000000000000000 ) ) ;
#15144 = DIRECTION ( 'NONE',  ( 1.000000000000000000, 0.000000000000000000, 0.000000000000000000 ) ) ;
#15145 = CARTESIAN_POINT ( 'NONE',  ( 0.07614184848677874040, 0.4941010236220472751, 0.000000000000000000 ) ) ;
#15146 = DIRECTION ( 'NONE',  ( -1.000000000000000000, 0.000000000000000000, 0.000000000000000000 ) ) ;
#15147 = ADVANCED_FACE ( 'NONE', ( #1406 ), #5660, .F. ) ;
#15148 = AXIS2_PLACEMENT_3D ( 'NONE', #13524, #22148, #19476 ) ;
#15149 = ADVANCED_FACE ( 'NONE', ( #20767, #10026 ), #16520, .T. ) ;
#15150 = CARTESIAN_POINT ( 'NONE',  ( 0.1623262587471781815, -0.4476804331129728975, 0.1212655228059691948 ) ) ;
#15151 = CARTESIAN_POINT ( 'NONE',  ( -0.09842519685039370636, 0.2165354330708661457, -3.272637795275590733 ) ) ;
#15152 = DIRECTION ( 'NONE',  ( 0.000000000000000000, -1.000000000000000000, 0.000000000000000000 ) ) ;
#15153 = AXIS2_PLACEMENT_3D ( 'NONE', #6799, #15430, #24022 ) ;
#15154 = CYLINDRICAL_SURFACE ( 'NONE', #17072, 0.3937007874015748254 ) ;
#15155 = B_SPLINE_CURVE_WITH_KNOTS ( 'NONE', 3,
 ( #16996, #23780, #25471, #21653, #10769, #342 ),
 .UNSPECIFIED., .F., .F.,
 ( 4, 2, 4 ),
 ( 0.5000000000000000000, 0.7500000000000000000, 1.000000000000000000 ),
 .UNSPECIFIED. ) ;
#15156 = FACE_OUTER_BOUND ( 'NONE', #17028, .T. ) ;
#15157 = CARTESIAN_POINT ( 'NONE',  ( -0.4783464566929133688, -0.4724409448818898127, -0.6411263657805729155 ) ) ;
#15158 = CARTESIAN_POINT ( 'NONE',  ( 0.4539000224941339701, 0.3482225189666781073, 0.9399606299212598381 ) ) ;
#15159 = FACE_OUTER_BOUND ( 'NONE', #10192, .T. ) ;
#15160 = ORIENTED_EDGE ( 'NONE', *, *, #7577, .F. ) ;
#15161 = DIRECTION ( 'NONE',  ( 0.000000000000000000, 0.000000000000000000, -1.000000000000000000 ) ) ;
#15162 = CIRCLE ( 'NONE', #2486, 0.3149606299212598381 ) ;
#15163 = ORIENTED_EDGE ( 'NONE', *, *, #6634, .F. ) ;
#15164 = VERTEX_POINT ( 'NONE', #16956 ) ;
#15165 = ORIENTED_EDGE ( 'NONE', *, *, #17447, .F. ) ;
#15166 = EDGE_CURVE ( 'NONE', #25001, #18714, #21043, .T. ) ;
#15167 = CARTESIAN_POINT ( 'NONE',  ( 0.4441657790094327707, -0.2564944395535760369, -1.550196850393700920 ) ) ;
#15168 = CARTESIAN_POINT ( 'NONE',  ( 0.000000000000000000, 0.000000000000000000, 0.1377952755905511861 ) ) ;
#15169 = AXIS2_PLACEMENT_3D ( 'NONE', #17784, #13138, #11570 ) ;
#15170 = CARTESIAN_POINT ( 'NONE',  ( 0.6751968503937006982, 8.268776616290199217E-17, -0.2618110236220472231 ) ) ;
#15171 = CARTESIAN_POINT ( 'NONE',  ( 0.2705157149885996093, -0.7122990885670630323, -8.723147988492308551E-17 ) ) ;
#15172 = EDGE_LOOP ( 'NONE', ( #6344, #7465, #17237, #7832 ) ) ;
#15173 = CARTESIAN_POINT ( 'NONE',  ( -0.2230788859036007821, 0.2650812153444458419, 0.1377952755905510474 ) ) ;
#15174 = AXIS2_PLACEMENT_3D ( 'NONE', #4576, #11210, #2455 ) ;
#15175 = CARTESIAN_POINT ( 'NONE',  ( -0.2983664441502653641, -0.6201464311010354002, 0.1322810039474933141 ) ) ;
#15176 = CARTESIAN_POINT ( 'NONE',  ( 0.1516263115863346334, 0.1971492568089271424, -0.4530651079966795947 ) ) ;
#15177 = DIRECTION ( 'NONE',  ( -0.000000000000000000, -1.000000000000000000, -0.000000000000000000 ) ) ;
#15178 = DIRECTION ( 'NONE',  ( 0.000000000000000000, 0.000000000000000000, -1.000000000000000000 ) ) ;
#15179 = CARTESIAN_POINT ( 'NONE',  ( 0.4895462770359960136, 1.042587244177305195, -0.2949132003431571003 ) ) ;
#15180 = ORIENTED_EDGE ( 'NONE', *, *, #26988, .T. ) ;
#15181 = DIRECTION ( 'NONE',  ( 0.000000000000000000, 0.000000000000000000, 1.000000000000000000 ) ) ;
#15182 = CARTESIAN_POINT ( 'NONE',  ( -0.3707612262532960501, 0.3252100150720461658, -1.550196850393700920 ) ) ;
#15183 = CARTESIAN_POINT ( 'NONE',  ( 0.4527559054764770385, 0.02963280468032115228, -1.934055118110236338 ) ) ;
#15184 = TOROIDAL_SURFACE ( 'NONE', #7497, 0.7883858267716535861, 0.05216535433070866590 ) ;
#15185 = CONICAL_SURFACE ( 'NONE', #6180, 0.1106489370078740098, 0.08726646250000029414 ) ;
#15186 = ORIENTED_EDGE ( 'NONE', *, *, #26961, .T. ) ;
#15187 = CARTESIAN_POINT ( 'NONE',  ( -0.6562077975700453258, 1.974383858267716320E-14, -0.07874015748031495954 ) ) ;
#15188 = CARTESIAN_POINT ( 'NONE',  ( 0.5905511811023621549, 0.000000000000000000, -0.3346456692913385988 ) ) ;
#15189 = CARTESIAN_POINT ( 'NONE',  ( 0.2355331214654088623, -0.4777261797697378021, 1.747047244094488194 ) ) ;
#15190 = CARTESIAN_POINT ( 'NONE',  ( -0.4895436826822647247, 0.08692528595283860460, 0.1615162260898340418 ) ) ;
#15191 = VERTEX_POINT ( 'NONE', #8198 ) ;
#15192 = EDGE_CURVE ( 'NONE', #9494, #13155, #12573, .T. ) ;
#15193 = FACE_OUTER_BOUND ( 'NONE', #18897, .T. ) ;
#15194 = CARTESIAN_POINT ( 'NONE',  ( -0.3520598332081320558, -0.04632226222358686724, 1.953740157480314821 ) ) ;
#15195 = CARTESIAN_POINT ( 'NONE',  ( 0.4333973147258542991, -0.2509079296564015737, 0.2574803149606298969 ) ) ;
#15196 = CARTESIAN_POINT ( 'NONE',  ( 0.2268599607409950980, -0.6212949646958005889, 0.1616495878780456474 ) ) ;
#15197 = EDGE_CURVE ( 'NONE', #13490, #27656, #25478, .T. ) ;
#15198 = ORIENTED_EDGE ( 'NONE', *, *, #11287, .T. ) ;
#15199 = CARTESIAN_POINT ( 'NONE',  ( -0.6722178168900768691, 0.05837462721528850068, 0.2350617247236460594 ) ) ;
#15200 = VERTEX_POINT ( 'NONE', #10299 ) ;
#15201 = CARTESIAN_POINT ( 'NONE',  ( -0.2761764805255799704, 0.3599896729929456529, -1.934055118110236338 ) ) ;
#15202 = PRODUCT_DEFINITION_FORMATION_WITH_SPECIFIED_SOURCE ( 'ANY', '', #3691, .NOT_KNOWN. ) ;
#15203 = CARTESIAN_POINT ( 'NONE',  ( 0.2428345617565153547, 0.2885915454824177218, 0.07637795275590551769 ) ) ;
#15204 = FACE_OUTER_BOUND ( 'NONE', #7614, .T. ) ;
#15205 = CARTESIAN_POINT ( 'NONE',  ( -0.4339912984563299436, -0.2498791196563492356, 0.09685039370078740717 ) ) ;
#15206 = EDGE_CURVE ( 'NONE', #25403, #27013, #4098, .T. ) ;
#15207 = AXIS2_PLACEMENT_3D ( 'NONE', #23309, #12684, #3936 ) ;
#15208 = CYLINDRICAL_SURFACE ( 'NONE', #27576, 0.1673228346456692994 ) ;
#15209 = CIRCLE ( 'NONE', #2982, 0.4941010236220472751 ) ;
#15210 = CARTESIAN_POINT ( 'NONE',  ( -0.2078289949484350141, -0.4330237525397957477, 0.2362204724409447676 ) ) ;
#15211 = CARTESIAN_POINT ( 'NONE',  ( 0.1200583359873109851, -0.3535721684717733071, -3.115157480314960647 ) ) ;
#15212 = DIRECTION ( 'NONE',  ( 0.000000000000000000, 1.000000000000000000, 0.000000000000000000 ) ) ;
#15213 = DIRECTION ( 'NONE',  ( 0.2588190448135648802, 0.000000000000000000, 0.9659258263664937116 ) ) ;
#15214 = CARTESIAN_POINT ( 'NONE',  ( -0.2490711204941346568, 0.7655264129003995777, -0.7689379837741201484 ) ) ;
#15215 = ORIENTED_EDGE ( 'NONE', *, *, #10157, .F. ) ;
#15216 = CARTESIAN_POINT ( 'NONE',  ( -0.3332647802741406373, -9.151579316449505861E-28, -0.1692378991623492424 ) ) ;
#15217 = ORIENTED_EDGE ( 'NONE', *, *, #2449, .T. ) ;
#15218 = CYLINDRICAL_SURFACE ( 'NONE', #15082, 0.1181102362204720091 ) ;
#15219 = CARTESIAN_POINT ( 'NONE',  ( 0.1518453843511950729, -0.2938239883646063255, 0.3972446186700991921 ) ) ;
#15220 = ORIENTED_EDGE ( 'NONE', *, *, #15556, .T. ) ;
#15221 = CIRCLE ( 'NONE', #16119, 1.988188976448617584 ) ;
#15222 = ORIENTED_EDGE ( 'NONE', *, *, #7803, .F. ) ;
#15223 = CARTESIAN_POINT ( 'NONE',  ( -0.3126261861395013275, 0.000000000000000000, -0.1464516454673935042 ) ) ;
#15224 = DIRECTION ( 'NONE',  ( 0.000000000000000000, 1.000000000000000000, 0.000000000000000000 ) ) ;
#15225 = CARTESIAN_POINT ( 'NONE',  ( -0.3855916753051397139, 0.3382184156732160329, 1.766732283464566899 ) ) ;
#15226 = LINE ( 'NONE', #17729, #8200 ) ;
#15227 = EDGE_CURVE ( 'NONE', #17614, #19912, #10392, .T. ) ;
#15228 = B_SPLINE_CURVE_WITH_KNOTS ( 'NONE', 3,
 ( #20114, #11499, #773, #5131, #14481, #22946 ),
 .UNSPECIFIED., .F., .F.,
 ( 4, 2, 4 ),
 ( 4.334600841719497663E-14, 0.0007294371397779656667, 0.001458874279512585364 ),
 .UNSPECIFIED. ) ;
#15229 = STYLED_ITEM ( 'NONE', ( #27342 ), #22049 ) ;
#15230 = ORIENTED_EDGE ( 'NONE', *, *, #6459, .F. ) ;
#15231 = CARTESIAN_POINT ( 'NONE',  ( -0.2962590301041646557, 0.2272836761397697136, -3.115157480314960647 ) ) ;
#15232 = ORIENTED_EDGE ( 'NONE', *, *, #11220, .F. ) ;
#15233 = ORIENTED_EDGE ( 'NONE', *, *, #19395, .T. ) ;
#15234 = CARTESIAN_POINT ( 'NONE',  ( 0.0006615832606325197825, 0.6212594902576319411, 0.09685039370078740717 ) ) ;
#15235 = SHAPE_REPRESENTATION_RELATIONSHIP ( 'NONE' , 'NONE' ,  #9188, #24457 ) ;
#15236 = FACE_OUTER_BOUND ( 'NONE', #7178, .T. ) ;
#15237 = EDGE_CURVE ( 'NONE', #333, #10134, #1833, .T. ) ;
#15238 = CARTESIAN_POINT ( 'NONE',  ( 0.2660793235464290474, -0.2041304421298306693, 1.953740157480315043 ) ) ;
#15239 = VERTEX_POINT ( 'NONE', #14856 ) ;
#15240 = VERTEX_POINT ( 'NONE', #21473 ) ;
#15241 = DIRECTION ( 'NONE',  ( -1.000000000000000000, 0.000000000000000000, 0.000000000000000000 ) ) ;
#15242 = ADVANCED_FACE ( 'NONE', ( #14988, #1970 ), #6223, .T. ) ;
#15243 = ORIENTED_EDGE ( 'NONE', *, *, #20264, .F. ) ;
#15244 = VERTEX_POINT ( 'NONE', #16816 ) ;
#15245 = EDGE_LOOP ( 'NONE', ( #21196, #19169, #16123, #5999, #10240, #18568 ) ) ;
#15246 = DIRECTION ( 'NONE',  ( -0.8176200022776350940, 0.000000000000000000, -0.5757582234545329802 ) ) ;
#15247 = ITEM_DEFINED_TRANSFORMATION ( 'NONE', 'NONE', #3911,  #11588 ) ;
#15248 = AXIS2_PLACEMENT_3D ( 'NONE', #10193, #20665, #18813 ) ;
#15249 = CARTESIAN_POINT ( 'NONE',  ( 0.4245040230929275626, 0.7010584879323878971, -0.6327280771288050776 ) ) ;
#15250 = CARTESIAN_POINT ( 'NONE',  ( -0.4055118110236220486, -0.4724409448818898127, -0.8182917201112815953 ) ) ;
#15251 = PRESENTATION_LAYER_ASSIGNMENT (  '', '', ( #16571 ) ) ;
#15252 = DIRECTION ( 'NONE',  ( 0.8660254037844385966, -0.4999999999999998335, 0.000000000000000000 ) ) ;
#15253 = ORIENTED_EDGE ( 'NONE', *, *, #7452, .T. ) ;
#15254 = PRODUCT_DEFINITION_SHAPE ( 'NONE', 'NONE',  #26544 ) ;
#15255 = ADVANCED_FACE ( 'NONE', ( #23470 ), #10579, .T. ) ;
#15256 = AXIS2_PLACEMENT_3D ( 'NONE', #7112, #7529, #3269 ) ;
#15257 = FACE_OUTER_BOUND ( 'NONE', #4332, .T. ) ;
#15258 = CARTESIAN_POINT ( 'NONE',  ( -0.1968503937007874127, -1.676732283464567127E-17, -0.09092130223458683158 ) ) ;
#15259 = ( CONVERSION_BASED_UNIT ( 'INCH', #22144 ) LENGTH_UNIT ( ) NAMED_UNIT ( #985 ) ) ;
#15260 = CARTESIAN_POINT ( 'NONE',  ( -0.3666644560843326239, 0.2817828961649161412, -1.928289503579156960 ) ) ;
#15261 = LINE ( 'NONE', #8341, #4698 ) ;
#15262 = DIRECTION ( 'NONE',  ( 0.000000000000000000, 0.000000000000000000, 1.000000000000000000 ) ) ;
#15263 = AXIS2_PLACEMENT_3D ( 'NONE', #23755, #21768, #4392 ) ;
#15264 = EDGE_CURVE ( 'NONE', #24998, #6679, #12208, .T. ) ;
#15265 = CARTESIAN_POINT ( 'NONE',  ( 0.09842519685039360922, 0.1968503937007873850, -3.272637795275590733 ) ) ;
#15266 = ORIENTED_EDGE ( 'NONE', *, *, #25931, .F. ) ;
#15267 = AXIS2_PLACEMENT_3D ( 'NONE', #3002, #13759, #9657 ) ;
#15268 = ORIENTED_EDGE ( 'NONE', *, *, #11269, .T. ) ;
#15269 = DIRECTION ( 'NONE',  ( 0.000000000000000000, 0.000000000000000000, -1.000000000000000000 ) ) ;
#15270 = EDGE_CURVE ( 'NONE', #16472, #5917, #16913, .T. ) ;
#15271 = EDGE_LOOP ( 'NONE', ( #24409, #4469 ) ) ;
#15272 = DIRECTION ( 'NONE',  ( 0.000000000000000000, 0.000000000000000000, -1.000000000000000000 ) ) ;
#15273 = STYLED_ITEM ( 'NONE', ( #23350 ), #21416 ) ;
#15274 = DIRECTION ( 'NONE',  ( 0.7071067818211432821, 0.000000000000000000, 0.7071067805519516414 ) ) ;
#15275 = CARTESIAN_POINT ( 'NONE',  ( -0.5636183736116697762, 1.118955382540468335, -0.03814816047951348488 ) ) ;
#15276 = CARTESIAN_POINT ( 'NONE',  ( -0.3924375359102375005, 0.3121297331111325124, 0.1643955689138890675 ) ) ;
#15277 = ORIENTED_EDGE ( 'NONE', *, *, #2389, .F. ) ;
#15278 = CARTESIAN_POINT ( 'NONE',  ( -0.2762247810519398716, 0.4783323773986303262, 0.9399606299212598381 ) ) ;
#15279 = VERTEX_POINT ( 'NONE', #5945 ) ;
#15280 = EDGE_CURVE ( 'NONE', #27454, #18611, #24544, .T. ) ;
#15281 = LINE ( 'NONE', #21763, #1411 ) ;
#15282 = EDGE_LOOP ( 'NONE', ( #9454, #27413 ) ) ;
#15283 = DIRECTION ( 'NONE',  ( 0.000000000000000000, 0.000000000000000000, 1.000000000000000000 ) ) ;
#15284 = CARTESIAN_POINT ( 'NONE',  ( 0.4164331889188472857, 0.3315254675241992577, 0.1322818204150988386 ) ) ;
#15285 = DIRECTION ( 'NONE',  ( -0.000000000000000000, -1.000000000000000000, -0.000000000000000000 ) ) ;
#15286 = DIRECTION ( 'NONE',  ( 0.000000000000000000, 1.000000000000000000, 0.000000000000000000 ) ) ;
#15287 = AXIS2_PLACEMENT_3D ( 'NONE', #20151, #26938, #20433 ) ;
#15288 = EDGE_CURVE ( 'NONE', #6278, #25761, #4705, .T. ) ;
#15289 = CIRCLE ( 'NONE', #21607, 0.6881889763779527325 ) ;
#15290 = ( BOUNDED_CURVE ( )  B_SPLINE_CURVE ( 2, ( #20635, #3234, #5811 ),
 .UNSPECIFIED., .F., .T. ) 
 B_SPLINE_CURVE_WITH_KNOTS ( ( 3, 3 ),
 ( 0.000000000000000000, 0.2336872276155829986 ),
 .UNSPECIFIED. ) 
 CURVE ( )  GEOMETRIC_REPRESENTATION_ITEM ( )  RATIONAL_B_SPLINE_CURVE ( ( 1.000000000000000000, 1.154700538379243913, 1.000000000000000000 ) ) 
 REPRESENTATION_ITEM ( '' )  ) ;
#15291 = FACE_OUTER_BOUND ( 'NONE', #20848, .T. ) ;
#15293 = CARTESIAN_POINT ( 'NONE',  ( 0.000000000000000000, 0.000000000000000000, 0.1377952755905511861 ) ) ;
#15292 = CIRCLE ( 'NONE', #11771, 0.5007874015748031704 ) ;
#15294 = CARTESIAN_POINT ( 'NONE',  ( -0.7283464566929135353, 8.919671568592928630E-17, 0.3425196850393700809 ) ) ;
#15295 = DIRECTION ( 'NONE',  ( -1.000000000000000000, 0.000000000000000000, 0.000000000000000000 ) ) ;
#15296 = VECTOR ( 'NONE', #17563, 39.37007874015748854 ) ;
#15297 = DIRECTION ( 'NONE',  ( 0.000000000000000000, 1.000000000000000000, 0.000000000000000000 ) ) ;
#15298 = CARTESIAN_POINT ( 'NONE',  ( 0.6202606299212598540, -6.779653543307085645E-20, 0.000000000000000000 ) ) ;
#15299 = FACE_OUTER_BOUND ( 'NONE', #5341, .T. ) ;
#15300 = CARTESIAN_POINT ( 'NONE',  ( 0.000000000000000000, 0.000000000000000000, 0.3543307086614173040 ) ) ;
#15301 = CARTESIAN_POINT ( 'NONE',  ( -0.1480156394741835579, -0.5526079293737254927, 0.9399606299212598381 ) ) ;
#15302 = VECTOR ( 'NONE', #22905, 39.37007874015748143 ) ;
#15303 = DIRECTION ( 'NONE',  ( 1.000000000000000000, 0.000000000000000000, 0.000000000000000000 ) ) ;
#15304 = ORIENTED_EDGE ( 'NONE', *, *, #9099, .T. ) ;
#15305 = CARTESIAN_POINT ( 'NONE',  ( 0.000000000000000000, 0.000000000000000000, -0.04133858267716535029 ) ) ;
#15306 = ADVANCED_FACE ( 'NONE', ( #27833 ), #20504, .T. ) ;
#15307 = B_SPLINE_CURVE_WITH_KNOTS ( 'NONE', 3,
 ( #25723, #21901, #15000, #4387, #23890, #27848 ),
 .UNSPECIFIED., .F., .F.,
 ( 4, 2, 4 ),
 ( 0.000000000000000000, 0.2500000000000000000, 0.5000000000000000000 ),
 .UNSPECIFIED. ) ;
#15308 = ORIENTED_EDGE ( 'NONE', *, *, #21159, .T. ) ;
#15309 = ORIENTED_EDGE ( 'NONE', *, *, #5907, .F. ) ;
#15310 = ADVANCED_FACE ( 'NONE', ( #17228 ), #1552, .T. ) ;
#15311 = AXIS2_PLACEMENT_3D ( 'NONE', #9695, #9260, #2905 ) ;
#15312 = ORIENTED_EDGE ( 'NONE', *, *, #12797, .T. ) ;
#15313 = ADVANCED_FACE ( 'NONE', ( #23180, #4631 ), #682, .T. ) ;
#15314 = CIRCLE ( 'NONE', #25656, 0.1298643763538141760 ) ;
#15315 = CARTESIAN_POINT ( 'NONE',  ( 0.4538399017589948015, -0.3483099419450786383, 0.9399606299212598381 ) ) ;
#15316 = DIRECTION ( 'NONE',  ( -1.224646799147353207E-16, 1.000000000000000000, 0.000000000000000000 ) ) ;
#15317 = AXIS2_PLACEMENT_3D ( 'NONE', #15598, #20091, #11070 ) ;
#15318 = CARTESIAN_POINT ( 'NONE',  ( 0.7874015748031496509, 3.035194737716535704E-06, -1.475314960619023674 ) ) ;
#15319 = DIRECTION ( 'NONE',  ( 0.9009688679024190350, -0.4338837391175581204, 0.000000000000000000 ) ) ;
#15320 = ORIENTED_EDGE ( 'NONE', *, *, #18798, .T. ) ;
#15321 = VERTEX_POINT ( 'NONE', #9272 ) ;
#15322 = LINE ( 'NONE', #15583, #26563 ) ;
#15323 = AXIS2_PLACEMENT_3D ( 'NONE', #26196, #19841, #498 ) ;
#15324 = FACE_OUTER_BOUND ( 'NONE', #18528, .T. ) ;
#15325 = CARTESIAN_POINT ( 'NONE',  ( -0.3998447049182095037, 0.4754871227241110332, 0.2574803149606298969 ) ) ;
#15326 = CARTESIAN_POINT ( 'NONE',  ( -0.4337933494688747671, -0.2502226818840338485, 0.2574827755769819038 ) ) ;
#15327 = DIRECTION ( 'NONE',  ( 0.000000000000000000, 1.000000000000000000, 0.000000000000000000 ) ) ;
#15328 = CARTESIAN_POINT ( 'NONE',  ( 0.000000000000000000, 0.07874015748031495954, 0.000000000000000000 ) ) ;
#15329 = CARTESIAN_POINT ( 'NONE',  ( -0.5393700787401575214, 6.605378404849898113E-17, 0.2637795275590551491 ) ) ;
#15330 = B_SPLINE_CURVE_WITH_KNOTS ( 'NONE', 3,
 ( #26727, #7383, #15133, #10304, #17095, #23609 ),
 .UNSPECIFIED., .F., .F.,
 ( 4, 2, 4 ),
 ( 0.000000000000000000, 0.2500000000000000000, 0.5000000000000000000 ),
 .UNSPECIFIED. ) ;
#15331 = ORIENTED_EDGE ( 'NONE', *, *, #8643, .F. ) ;
#15332 = CARTESIAN_POINT ( 'NONE',  ( 0.03189995399141003218, 0.3133994105366679772, -3.641567849138989121 ) ) ;
#15333 = CARTESIAN_POINT ( 'NONE',  ( -0.08530183727034117147, -0.03937007874015755610, -0.06819097667594038736 ) ) ;
#15334 = CARTESIAN_POINT ( 'NONE',  ( 0.3707612262533330205, 0.3252100150720381722, -1.550196850393700920 ) ) ;
#15335 = AXIS2_PLACEMENT_3D ( 'NONE', #25933, #23555, #2696 ) ;
#15336 = CARTESIAN_POINT ( 'NONE',  ( 0.1477428134820460426, 0.4351030398461616100, -1.928289503579165842 ) ) ;
#15337 = AXIS2_PLACEMENT_3D ( 'NONE', #17682, #13043, #4691 ) ;
#15338 = AXIS2_PLACEMENT_3D ( 'NONE', #16543, #18946, #20934 ) ;
#15339 = CARTESIAN_POINT ( 'NONE',  ( 0.2311492806687369950, -0.4794744477484330636, 0.3401599409343964431 ) ) ;
#15340 = CARTESIAN_POINT ( 'NONE',  ( -0.5375739373539409893, 0.4296723508511055556, 0.1322834645669291320 ) ) ;
#15341 = CONICAL_SURFACE ( 'NONE', #2656, 1.112204724409448842, 0.7853981624999977207 ) ;
#15342 = DIRECTION ( 'NONE',  ( 0.7818314824680296926, -0.6234898018587338164, 0.000000000000000000 ) ) ;
#15343 = CARTESIAN_POINT ( 'NONE',  ( -0.07874015748031502893, 0.1968503937007874127, -3.272637795275590733 ) ) ;
#15344 = ADVANCED_FACE ( 'NONE', ( #2516 ), #4371, .F. ) ;
#15345 = ORIENTED_EDGE ( 'NONE', *, *, #14669, .T. ) ;
#15346 = CARTESIAN_POINT ( 'NONE',  ( -0.07874015748031495954, -1.062017969535966354E-23, -0.4653543306978102367 ) ) ;
#15347 = CARTESIAN_POINT ( 'NONE',  ( -0.6299212598425196763, -0.6348133144914134274, 0.8891632684400255782 ) ) ;
#15348 = ORIENTED_EDGE ( 'NONE', *, *, #20542, .T. ) ;
#15349 = CARTESIAN_POINT ( 'NONE',  ( 0.000000000000000000, 0.000000000000000000, 0.1771653543307086520 ) ) ;
#15350 = EDGE_LOOP ( 'NONE', ( #16627, #20410, #18524, #19611, #7709, #4731, #4594, #26210, #14434, #22168, #18740, #18136, #23909, #14188, #25969, #22649 ) ) ;
#15351 = CIRCLE ( 'NONE', #20726, 0.7165354330708662012 ) ;
#15352 = CARTESIAN_POINT ( 'NONE',  ( 2.186367668367731174E-17, 0.3771653543307086909, 0.1992150590373740204 ) ) ;
#15353 = ORIENTED_EDGE ( 'NONE', *, *, #14418, .F. ) ;
#15354 = CARTESIAN_POINT ( 'NONE',  ( -0.2006393256663633884, 0.4069519308876736741, -1.934055118110236338 ) ) ;
#15355 = CARTESIAN_POINT ( 'NONE',  ( 0.2425693455392318731, 0.2888145544500153594, 0.07637549214372835182 ) ) ;
#15356 = AXIS2_PLACEMENT_3D ( 'NONE', #21808, #102, #2301 ) ;
#15357 = DIRECTION ( 'NONE',  ( 0.000000000000000000, 0.000000000000000000, -1.000000000000000000 ) ) ;
#15358 = CARTESIAN_POINT ( 'NONE',  ( 0.3102399269716953345, -1.154980647406259830, -0.4411320940076480235 ) ) ;
#15359 = CARTESIAN_POINT ( 'NONE',  ( 2.664928230027803213, -0.4724409448818898127, -0.8182917201112815953 ) ) ;
#15360 = CARTESIAN_POINT ( 'NONE',  ( -0.2712695779734264900, -0.3534635626045726786, -1.934055118110236116 ) ) ;
#15361 = CARTESIAN_POINT ( 'NONE',  ( 0.3702005978258584573, 0.04877294052296160531, -3.115157480314960647 ) ) ;
#15362 = CARTESIAN_POINT ( 'NONE',  ( 0.7874015748031496509, 0.000000000000000000, -1.052618110236220428 ) ) ;
#15363 = DIRECTION ( 'NONE',  ( 1.000000000000000000, 0.000000000000000000, 0.000000000000000000 ) ) ;
#15364 = DIRECTION ( 'NONE',  ( -1.000000000000000000, 0.000000000000000000, 0.000000000000000000 ) ) ;
#15365 = EDGE_CURVE ( 'NONE', #7957, #27881, #11936, .T. ) ;
#15366 = ORIENTED_EDGE ( 'NONE', *, *, #17665, .T. ) ;
#15367 = ADVANCED_FACE ( 'NONE', ( #4511 ), #12979, .T. ) ;
#15368 = CARTESIAN_POINT ( 'NONE',  ( -0.4218945342797432163, 0.1432577568504689591, -1.934055118110236338 ) ) ;
#15369 = VECTOR ( 'NONE', #24153, 39.37007874015748854 ) ;
#15370 = CIRCLE ( 'NONE', #2250, 0.7480314960629921295 ) ;
#15371 = ORIENTED_EDGE ( 'NONE', *, *, #4375, .F. ) ;
#15372 = ADVANCED_FACE ( 'NONE', ( #17885 ), #5143, .T. ) ;
#15373 = ADVANCED_FACE ( 'NONE', ( #173 ), #21745, .F. ) ;
#15374 = CARTESIAN_POINT ( 'NONE',  ( 0.4684132450478833976, -0.1062614382955264641, 0.2362204724409446843 ) ) ;
#15375 = CARTESIAN_POINT ( 'NONE',  ( -5.747161356628524594E-17, -0.4692913385826771866, 0.03818897637795275884 ) ) ;
#15376 = CARTESIAN_POINT ( 'NONE',  ( 0.000000000000000000, 0.000000000000000000, -0.1309055118110236116 ) ) ;
#15377 = PLANE ( 'NONE',  #10425 ) ;
#15378 = EDGE_LOOP ( 'NONE', ( #3921, #13867 ) ) ;
#15379 = AXIS2_PLACEMENT_3D ( 'NONE', #1420, #25152, #10035 ) ;
#15380 = VERTEX_POINT ( 'NONE', #4912 ) ;
#15381 = CARTESIAN_POINT ( 'NONE',  ( -0.2272836761397795113, -0.2962590301041581053, -3.115157480314960647 ) ) ;
#15382 = ORIENTED_EDGE ( 'NONE', *, *, #5207, .T. ) ;
#15383 = DIRECTION ( 'NONE',  ( -1.000000000000000000, 0.000000000000000000, 0.000000000000000000 ) ) ;
#15384 = CARTESIAN_POINT ( 'NONE',  ( 0.000000000000000000, 0.000000000000000000, 0.000000000000000000 ) ) ;
#15385 = CARTESIAN_POINT ( 'NONE',  ( 0.06200787401574745644, 0.000000000000000000, -4.209669677817527322 ) ) ;
#15386 = CARTESIAN_POINT ( 'NONE',  ( -0.2904160862623610950, -0.1677079028045287690, 1.953740157480315043 ) ) ;
#15387 = ORIENTED_EDGE ( 'NONE', *, *, #871, .T. ) ;
#15388 = ORIENTED_EDGE ( 'NONE', *, *, #1948, .F. ) ;
#15389 = DIRECTION ( 'NONE',  ( 1.000000000000000000, 0.000000000000000000, 0.000000000000000000 ) ) ;
#15390 = ORIENTED_EDGE ( 'NONE', *, *, #24463, .F. ) ;
#15391 = ORIENTED_EDGE ( 'NONE', *, *, #24463, .T. ) ;
#15392 = DIRECTION ( 'NONE',  ( 0.000000000000000000, 0.000000000000000000, -1.000000000000000000 ) ) ;
#15393 = EDGE_LOOP ( 'NONE', ( #26059, #22263, #156, #10406 ) ) ;
#15394 = CIRCLE ( 'NONE', #24365, 0.7283464566929134243 ) ;
#15395 = CARTESIAN_POINT ( 'NONE',  ( 0.4895462770359960136, 0.9151958316344488420, -0.3874954751609366310 ) ) ;
#15396 = DIRECTION ( 'NONE',  ( -1.000000000000000000, 0.000000000000000000, 0.000000000000000000 ) ) ;
#15397 = CARTESIAN_POINT ( 'NONE',  ( 0.6141002140709024282, 0.8998311997009023067, -0.1298280283246295574 ) ) ;
#15398 = EDGE_CURVE ( 'NONE', #19875, #27874, #7505, .T. ) ;
#15399 = CIRCLE ( 'NONE', #10382, 0.6881889763779527325 ) ;
#15400 = CARTESIAN_POINT ( 'NONE',  ( -0.1968503937007874127, 0.1291220684401279684, 0.000000000000000000 ) ) ;
#15401 = EDGE_CURVE ( 'NONE', #3555, #14474, #1553, .T. ) ;
#15402 = ADVANCED_FACE ( 'NONE', ( #426, #10862 ), #26381, .F. ) ;
#15403 = CARTESIAN_POINT ( 'NONE',  ( -0.5675505653814777451, 1.114319256831761251, 0.05180297602549875646 ) ) ;
#15404 = EDGE_CURVE ( 'NONE', #26363, #22611, #21868, .T. ) ;
#15405 = B_SPLINE_CURVE_WITH_KNOTS ( 'NONE', 3,
 ( #354, #24051, #23340, #474, #95, #8660 ),
 .UNSPECIFIED., .F., .F.,
 ( 4, 2, 4 ),
 ( 0.3000437156586439613, 0.3015484798814569989, 0.3030532441042709801 ),
 .UNSPECIFIED. ) ;
#15406 = DIRECTION ( 'NONE',  ( -1.000000000000000000, 0.000000000000000000, 0.000000000000000000 ) ) ;
#15407 = CARTESIAN_POINT ( 'NONE',  ( 0.000000000000000000, 0.000000000000000000, 0.1771653543307086520 ) ) ;
#15408 = CARTESIAN_POINT ( 'NONE',  ( -9.069736220472442904E-16, -0.8267716535433071723, -0.7883858267716535861 ) ) ;
#15409 = AXIS2_PLACEMENT_3D ( 'NONE', #3899, #9832, #9691 ) ;
#15410 = CARTESIAN_POINT ( 'NONE',  ( -0.09842519685039373412, 0.1968503937007873850, -3.272637795275590733 ) ) ;
#15411 = EDGE_LOOP ( 'NONE', ( #18247, #640, #25105, #19674 ) ) ;
#15412 = FACE_OUTER_BOUND ( 'NONE', #7327, .T. ) ;
#15413 = ADVANCED_FACE ( 'NONE', ( #15665, #13118 ), #24263, .F. ) ;
#15414 = CARTESIAN_POINT ( 'NONE',  ( 0.2669897767697305135, -0.2341075107470857453, 1.953740157480315043 ) ) ;
#15415 = ORIENTED_EDGE ( 'NONE', *, *, #14302, .T. ) ;
#15416 = DIRECTION ( 'NONE',  ( 1.000000000000000000, 0.000000000000000000, 0.000000000000000000 ) ) ;
#15417 = CONICAL_SURFACE ( 'NONE', #13566, 0.08582677165393072516, 0.7853981625000011624 ) ;
#15418 = CARTESIAN_POINT ( 'NONE',  ( 0.000000000000000000, 0.000000000000000000, -3.278217716535432842E-17 ) ) ;
#15419 = CARTESIAN_POINT ( 'NONE',  ( 0.000000000000000000, 0.6212598425196850238, 0.3059055118110236560 ) ) ;
#15420 = CYLINDRICAL_SURFACE ( 'NONE', #14384, 0.6889763779527560139 ) ;
#15421 = ORIENTED_EDGE ( 'NONE', *, *, #19986, .T. ) ;
#15422 = CARTESIAN_POINT ( 'NONE',  ( -0.2442565704126265502, 0.4954197419817717996, 0.9399606299212598381 ) ) ;
#15423 = DIRECTION ( 'NONE',  ( 0.000000000000000000, 1.000000000000000000, 0.000000000000000000 ) ) ;
#15424 = LINE ( 'NONE', #25864, #12704 ) ;
#15425 = CARTESIAN_POINT ( 'NONE',  ( 0.1632039128460986976, -0.4501088385473325237, 0.08349695147770751225 ) ) ;
#15426 = CARTESIAN_POINT ( 'NONE',  ( -0.3661417322834645272, -0.4724409448818898127, 0.9954570744419902750 ) ) ;
#15427 = CARTESIAN_POINT ( 'NONE',  ( 0.2979095355690402069, -0.6203660015065080024, 0.1322834645669291320 ) ) ;
#15428 = EDGE_CURVE ( 'NONE', #25987, #10805, #3363, .T. ) ;
#15429 = CARTESIAN_POINT ( 'NONE',  ( 0.6711032387266614441, -0.1523958994813204848, 0.1322834645669291320 ) ) ;
#15430 = DIRECTION ( 'NONE',  ( -1.000000000000000000, 0.000000000000000000, 0.000000000000000000 ) ) ;
#15431 = CARTESIAN_POINT ( 'NONE',  ( 0.4925073816792371884, 0.08623502184977957508, 0.1496602734459366590 ) ) ;
#15432 = CARTESIAN_POINT ( 'NONE',  ( 0.000000000000000000, 0.000000000000000000, 0.1377952755905511584 ) ) ;
#15433 = EDGE_CURVE ( 'NONE', #12691, #7184, #22782, .T. ) ;
#15434 = FACE_OUTER_BOUND ( 'NONE', #26257, .T. ) ;
#15435 = AXIS2_PLACEMENT_3D ( 'NONE', #24368, #24924, #5584 ) ;
#15436 = CARTESIAN_POINT ( 'NONE',  ( -0.07472527936312116370, 0.5671862884094760471, 0.9399606299212598381 ) ) ;
#15437 = ORIENTED_EDGE ( 'NONE', *, *, #21075, .T. ) ;
#15438 = DIRECTION ( 'NONE',  ( 0.000000000000000000, 0.000000000000000000, -1.000000000000000000 ) ) ;
#15439 = CARTESIAN_POINT ( 'NONE',  ( 0.4898768902087983768, 0.000000000000000000, -0.2362204724409449064 ) ) ;
#15440 = CARTESIAN_POINT ( 'NONE',  ( -0.3574975638436101444, 0.000000000000000000, -3.115157480314960647 ) ) ;
#15441 = EDGE_CURVE ( 'NONE', #19404, #12816, #16938, .T. ) ;
#15442 = ORIENTED_EDGE ( 'NONE', *, *, #2778, .T. ) ;
#15443 = VERTEX_POINT ( 'NONE', #8203 ) ;
#15444 = CIRCLE ( 'NONE', #26247, 0.06200787401574745644 ) ;
#15445 = CARTESIAN_POINT ( 'NONE',  ( -0.3338887748335570560, -1.036595354089161480, -0.8696564807123209340 ) ) ;
#15446 = CARTESIAN_POINT ( 'NONE',  ( 0.03008364706454716778, -0.1136516277932334562, 0.1968503937007874127 ) ) ;
#15447 = FACE_OUTER_BOUND ( 'NONE', #1776, .T. ) ;
#15448 = ORIENTED_EDGE ( 'NONE', *, *, #20028, .T. ) ;
#15449 = DIRECTION ( 'NONE',  ( 0.000000000000000000, 1.000000000000000000, 0.000000000000000000 ) ) ;
#15450 = VERTEX_POINT ( 'NONE', #21197 ) ;
#15451 = CYLINDRICAL_SURFACE ( 'NONE', #5790, 0.4692913385826771866 ) ;
#15452 = CARTESIAN_POINT ( 'NONE',  ( 0.6711032387266614441, -0.1523958994813204848, 0.1322834645669291320 ) ) ;
#15453 = DIRECTION ( 'NONE',  ( 0.000000000000000000, 0.000000000000000000, 1.000000000000000000 ) ) ;
#15454 = EDGE_CURVE ( 'NONE', #12305, #17515, #25144, .T. ) ;
#15455 = CARTESIAN_POINT ( 'NONE',  ( -0.03937007874015747977, 0.000000000000000000, 0.000000000000000000 ) ) ;
#15456 = VERTEX_POINT ( 'NONE', #23335 ) ;
#15457 = LINE ( 'NONE', #17417, #11646 ) ;
#15458 = CARTESIAN_POINT ( 'NONE',  ( 0.4669911931914377257, 0.1585706980422264545, -1.550196850393700920 ) ) ;
#15459 = EDGE_CURVE ( 'NONE', #26519, #23791, #18241, .T. ) ;
#15460 = CONICAL_SURFACE ( 'NONE', #19047, 0.2012500529900838608, 1.047197550000000144 ) ;
#15461 = CARTESIAN_POINT ( 'NONE',  ( -0.1188866373884864824, -0.4438564651657386229, -1.928289503579162067 ) ) ;
#15462 = CIRCLE ( 'NONE', #3233, 0.4692913385826771866 ) ;
#15463 = CARTESIAN_POINT ( 'NONE',  ( -0.5510854067032040504, 0.4384931681280017091, 0.1443310008628239383 ) ) ;
#15464 = FACE_OUTER_BOUND ( 'NONE', #7181, .T. ) ;
#15465 = AXIS2_PLACEMENT_3D ( 'NONE', #26535, #1367, #3611 ) ;
#15466 = ORIENTED_EDGE ( 'NONE', *, *, #19409, .T. ) ;
#15467 = CARTESIAN_POINT ( 'NONE',  ( -0.6208708315385689236, -0.1114655006168945028, 0.07327095640358681494 ) ) ;
#15468 = DIRECTION ( 'NONE',  ( -1.000000000000000000, 0.000000000000000000, 0.000000000000000000 ) ) ;
#15469 = DIRECTION ( 'NONE',  ( 0.000000000000000000, 1.000000000000000000, 0.000000000000000000 ) ) ;
#15470 = VERTEX_POINT ( 'NONE', #27412 ) ;
#15471 = EDGE_CURVE ( 'NONE', #20711, #798, #13204, .T. ) ;
#15472 = CARTESIAN_POINT ( 'NONE',  ( -0.07874015748031495954, 0.02870882010207796015, -0.4702759304817425434 ) ) ;
#15473 = DIRECTION ( 'NONE',  ( -0.000000000000000000, -1.000000000000000000, -0.000000000000000000 ) ) ;
#15474 = VERTEX_POINT ( 'NONE', #20772 ) ;
#15475 = PRODUCT_DEFINITION_SHAPE ( 'NONE', 'NONE',  #27891 ) ;
#15476 = LINE ( 'NONE', #4712, #6433 ) ;
#15477 = DIRECTION ( 'NONE',  ( 0.000000000000000000, -1.000000000000000000, 0.000000000000000000 ) ) ;
#15478 = AXIS2_PLACEMENT_3D ( 'NONE', #20670, #24899, #7533 ) ;
#15479 = CARTESIAN_POINT ( 'NONE',  ( -0.6806799598997224088, 0.05663649493104071925, -0.2380830294301988226 ) ) ;
#15480 = ORIENTED_EDGE ( 'NONE', *, *, #13968, .F. ) ;
#15481 = CIRCLE ( 'NONE', #12762, 0.7283464566929134243 ) ;
#15482 = CARTESIAN_POINT ( 'NONE',  ( 0.000000000000000000, 0.000000000000000000, -0.3779527559055118058 ) ) ;
#15483 = DIRECTION ( 'NONE',  ( 1.000000000000000000, 0.000000000000000000, 0.000000000000000000 ) ) ;
#15484 = CARTESIAN_POINT ( 'NONE',  ( 0.0005939837304750000086, 0.5007870493127504208, 0.09685039370078740717 ) ) ;
#15485 = AXIS2_PLACEMENT_3D ( 'NONE', #10329, #23496, #21501 ) ;
#15486 = CARTESIAN_POINT ( 'NONE',  ( -2.685748425196850164E-17, 0.000000000000000000, -3.745078740157480546 ) ) ;
#15487 = CARTESIAN_POINT ( 'NONE',  ( 0.1213180142433833847, 0.3572819248074460829, -3.100567304031761395 ) ) ;
#15488 = CARTESIAN_POINT ( 'NONE',  ( 0.1522836969735573143, 0.000000000000000000, 0.000000000000000000 ) ) ;
#15489 = DIRECTION ( 'NONE',  ( -1.000000000000000000, 0.000000000000000000, 0.000000000000000000 ) ) ;
#15490 = DIRECTION ( 'NONE',  ( 0.000000000000000000, 0.000000000000000000, -1.000000000000000000 ) ) ;
#15491 = EDGE_CURVE ( 'NONE', #13154, #21686, #19960, .T. ) ;
#15492 = ORIENTED_EDGE ( 'NONE', *, *, #13797, .T. ) ;
#15493 = DIRECTION ( 'NONE',  ( -1.000000000000000000, 0.000000000000000000, 0.000000000000000000 ) ) ;
#15494 = B_SPLINE_CURVE_WITH_KNOTS ( 'NONE', 2,
 ( #11300, #26004, #704 ),
 .UNSPECIFIED., .F., .F.,
 ( 3, 3 ),
 ( 0.000000000000000000, 1.000000000000000000 ),
 .UNSPECIFIED. ) ;
#15495 = CONICAL_SURFACE ( 'NONE', #16844, 0.4055307389460929279, 0.3230892413134540120 ) ;
#15496 = CIRCLE ( 'NONE', #6479, 0.4173228346456693272 ) ;
#15497 = ORIENTED_EDGE ( 'NONE', *, *, #3325, .T. ) ;
#15498 = EDGE_CURVE ( 'NONE', #18835, #4773, #5169, .T. ) ;
#15499 = LINE ( 'NONE', #17855, #27756 ) ;
#15500 = CARTESIAN_POINT ( 'NONE',  ( -0.06699590632655402778, 0.5118110236220472231, 1.766732283464566899 ) ) ;
#15501 = AXIS2_PLACEMENT_3D ( 'NONE', #23441, #14830, #25820 ) ;
#15502 = CARTESIAN_POINT ( 'NONE',  ( 0.2268096725222696064, 0.4600326175561003650, 1.747047244094488194 ) ) ;
#15503 = CARTESIAN_POINT ( 'NONE',  ( 2.632951206231566310, 0.9448818897637796255, -9.561468503937007847E-18 ) ) ;
#15504 = ORIENTED_EDGE ( 'NONE', *, *, #7108, .T. ) ;
#15505 = VERTEX_POINT ( 'NONE', #26221 ) ;
#15507 = CARTESIAN_POINT ( 'NONE',  ( -0.1651192144506243575, -0.3349073414798197645, -3.115157480314960647 ) ) ;
#15506 = CARTESIAN_POINT ( 'NONE',  ( -0.6339803004471820103, 0.1124719464481696296, 0.2359405056191490324 ) ) ;
#15508 = AXIS2_PLACEMENT_3D ( 'NONE', #24527, #3043, #26374 ) ;
#15509 = ORIENTED_EDGE ( 'NONE', *, *, #14128, .F. ) ;
#15510 = FACE_OUTER_BOUND ( 'NONE', #7650, .T. ) ;
#15511 = DIRECTION ( 'NONE',  ( 0.000000000000000000, 0.000000000000000000, -1.000000000000000000 ) ) ;
#15512 = EDGE_LOOP ( 'NONE', ( #11084, #22781, #14346, #6796 ) ) ;
#15513 = CARTESIAN_POINT ( 'NONE',  ( 0.2211428102655656758, 0.2521176338356670432, 1.953740157480315043 ) ) ;
#15514 = ORIENTED_EDGE ( 'NONE', *, *, #1754, .F. ) ;
#15516 = ADVANCED_FACE ( 'NONE', ( #2749 ), #1141, .F. ) ;
#15515 = ORIENTED_EDGE ( 'NONE', *, *, #10225, .T. ) ;
#15517 = EDGE_LOOP ( 'NONE', ( #16337, #513, #6866, #2473 ) ) ;
#15518 = CARTESIAN_POINT ( 'NONE',  ( -0.3149606299212598381, 0.000000000000000000, 0.000000000000000000 ) ) ;
#15519 = ORIENTED_EDGE ( 'NONE', *, *, #3755, .F. ) ;
#15520 = ORIENTED_EDGE ( 'NONE', *, *, #3631, .T. ) ;
#15521 = CARTESIAN_POINT ( 'NONE',  ( 0.07874015748031495954, 0.1968503937007874127, -3.548228346456692162 ) ) ;
#15522 = AXIS2_PLACEMENT_3D ( 'NONE', #7106, #9337, #893 ) ;
#15523 = AXIS2_PLACEMENT_3D ( 'NONE', #16934, #23849, #13096 ) ;
#15524 = EDGE_CURVE ( 'NONE', #4649, #27798, #3833, .T. ) ;
#15525 = CARTESIAN_POINT ( 'NONE',  ( -0.5177165354330708347, 0.9448818897637796255, 0.1771653543307086520 ) ) ;
#15526 = CARTESIAN_POINT ( 'NONE',  ( 0.000000000000000000, 0.000000000000000000, 0.1377952755905511861 ) ) ;
#15527 = DIRECTION ( 'NONE',  ( 0.000000000000000000, 1.000000000000000000, 0.000000000000000000 ) ) ;
#15528 = FACE_BOUND ( 'NONE', #3415, .T. ) ;
#15529 = CONTEXT_DEPENDENT_SHAPE_REPRESENTATION ( #14542, #18386 ) ;
#15530 = AXIS2_PLACEMENT_3D ( 'NONE', #10023, #3809, #12428 ) ;
#15531 = CARTESIAN_POINT ( 'NONE',  ( -0.2118615749922956593, -0.5840192333899354438, 0.09685039370078740717 ) ) ;
#15532 = DIRECTION ( 'NONE',  ( 0.000000000000000000, 1.000000000000000000, 0.000000000000000000 ) ) ;
#15533 = CARTESIAN_POINT ( 'NONE',  ( -0.1771653543307086520, -5.663984251968503442E-18, 0.000000000000000000 ) ) ;
#15534 = CARTESIAN_POINT ( 'NONE',  ( 0.0006345105826664493992, 0.4803145415259079121, 0.2362204724409449896 ) ) ;
#15535 = CARTESIAN_POINT ( 'NONE',  ( -0.06699507805369007973, 0.5085118447801436625, 1.766732283464566899 ) ) ;
#15536 = CIRCLE ( 'NONE', #1990, 1.288838582677165778 ) ;
#15537 = EDGE_CURVE ( 'NONE', #7099, #24215, #2186, .T. ) ;
#15538 = DIRECTION ( 'NONE',  ( 0.000000000000000000, -1.000000000000000000, 0.000000000000000000 ) ) ;
#15539 = ORIENTED_EDGE ( 'NONE', *, *, #2085, .T. ) ;
#15540 = LINE ( 'NONE', #11693, #10994 ) ;
#15541 = CARTESIAN_POINT ( 'NONE',  ( 0.1775236553383016391, -0.3075341118175515809, 1.953740157480314821 ) ) ;
#15542 = VERTEX_POINT ( 'NONE', #8546 ) ;
#15543 = DIRECTION ( 'NONE',  ( 0.000000000000000000, 1.000000000000000000, 0.000000000000000000 ) ) ;
#15544 = EDGE_CURVE ( 'NONE', #16265, #6630, #11960, .T. ) ;
#15545 = AXIS2_PLACEMENT_3D ( 'NONE', #1036, #25032, #26869 ) ;
#15546 = DIRECTION ( 'NONE',  ( 0.000000000000000000, 0.000000000000000000, -1.000000000000000000 ) ) ;
#15547 = CARTESIAN_POINT ( 'NONE',  ( 0.4456396174367268093, 5.674725427529967790E-17, -0.1696422624804970747 ) ) ;
#15548 = VECTOR ( 'NONE', #25045, 39.37007874015748143 ) ;
#15549 = ORIENTED_EDGE ( 'NONE', *, *, #825, .T. ) ;
#15550 = CARTESIAN_POINT ( 'NONE',  ( 0.4152525734086270348, -0.3642352168757560515, 0.9202755905511811330 ) ) ;
#15551 = VERTEX_POINT ( 'NONE', #8272 ) ;
#15552 = EDGE_CURVE ( 'NONE', #15164, #15630, #6181, .T. ) ;
#15553 = DIRECTION ( 'NONE',  ( -1.000000000000000000, 0.000000000000000000, 0.000000000000000000 ) ) ;
#15554 = ORIENTED_EDGE ( 'NONE', *, *, #7763, .F. ) ;
#15555 = ( NAMED_UNIT ( * ) SI_UNIT ( $, .STERADIAN. ) SOLID_ANGLE_UNIT ( ) ) ;
#15556 = EDGE_CURVE ( 'NONE', #158, #24837, #26323, .T. ) ;
#15557 = CARTESIAN_POINT ( 'NONE',  ( 0.000000000000000000, 0.1968503937007875237, 0.000000000000000000 ) ) ;
#15558 = CARTESIAN_POINT ( 'NONE',  ( 0.3180687940157840843, -3.895219305000888202E-17, -0.04133858267716535029 ) ) ;
#15559 = SPHERICAL_SURFACE ( 'NONE', #19184, 0.07677362204724409722 ) ;
#15560 = CIRCLE ( 'NONE', #5627, 0.4685039370078740717 ) ;
#15561 = DIRECTION ( 'NONE',  ( 0.000000000000000000, 0.000000000000000000, 1.000000000000000000 ) ) ;
#15562 = CYLINDRICAL_SURFACE ( 'NONE', #5193, 0.3937007874015748254 ) ;
#15563 = CARTESIAN_POINT ( 'NONE',  ( 0.000000000000000000, 0.000000000000000000, 0.3425196850393700809 ) ) ;
#15564 = CARTESIAN_POINT ( 'NONE',  ( -0.4061284506583976994, -0.2351468520617070734, 0.1992125984251968684 ) ) ;
#15565 = DIRECTION ( 'NONE',  ( -1.000000000000000000, 0.000000000000000000, 0.000000000000000000 ) ) ;
#15566 = DIRECTION ( 'NONE',  ( -1.000000000000000000, 0.000000000000000000, 0.000000000000000000 ) ) ;
#15567 = CARTESIAN_POINT ( 'NONE',  ( 0.03736310157557471562, -0.5708661417322835607, 0.9399606299212598381 ) ) ;
#15568 = CARTESIAN_POINT ( 'NONE',  ( 0.5118110236220471121, -0.06699590632655400002, 1.766732283464566899 ) ) ;
#15569 = CIRCLE ( 'NONE', #7435, 0.3332647802741406373 ) ;
#15570 = DIRECTION ( 'NONE',  ( 1.000000000000000000, 0.000000000000000000, 0.000000000000000000 ) ) ;
#15571 = CARTESIAN_POINT ( 'NONE',  ( 1.687505431895960050E-16, 0.4724409448818898127, -1.377952755905512472 ) ) ;
#15572 = ADVANCED_FACE ( 'NONE', ( #4709 ), #14700, .F. ) ;
#15573 = CIRCLE ( 'NONE', #10593, 0.4692913385826771866 ) ;
#15574 = ORIENTED_EDGE ( 'NONE', *, *, #9288, .F. ) ;
#15575 = DIRECTION ( 'NONE',  ( 0.000000000000000000, 0.000000000000000000, -1.000000000000000000 ) ) ;
#15576 = DIRECTION ( 'NONE',  ( 1.000000000000000000, 0.000000000000000000, 0.000000000000000000 ) ) ;
#15577 = CARTESIAN_POINT ( 'NONE',  ( 9.642888182262624280E-17, 0.3543307086614173040, 0.7874015748031496509 ) ) ;
#15578 = ORIENTED_EDGE ( 'NONE', *, *, #1109, .T. ) ;
#15579 = EDGE_CURVE ( 'NONE', #17370, #4618, #8788, .T. ) ;
#15580 = CARTESIAN_POINT ( 'NONE',  ( 0.1490609433576163545, -0.2393035190829114200, 0.4144858534816307505 ) ) ;
#15581 = EDGE_LOOP ( 'NONE', ( #19424, #12580, #16046, #9826, #2957, #2895 ) ) ;
#15582 = AXIS2_PLACEMENT_3D ( 'NONE', #17727, #7011, #395 ) ;
#15583 = CARTESIAN_POINT ( 'NONE',  ( -1.692913385826771533, 0.07874015748031495954, -0.1181102362204721062 ) ) ;
#15584 = CIRCLE ( 'NONE', #25518, 0.5511811023622047445 ) ;
#15585 = CARTESIAN_POINT ( 'NONE',  ( 0.4895462770358314786, 0.6591390924234138415, -0.5735858475448201155 ) ) ;
#15586 = LINE ( 'NONE', #19541, #1735 ) ;
#15587 = ADVANCED_FACE ( 'NONE', ( #18452 ), #9693, .F. ) ;
#15588 = CARTESIAN_POINT ( 'NONE',  ( -8.427884271297532088E-17, -0.6881889763779527325, 0.1322834645669291320 ) ) ;
#15589 = EDGE_CURVE ( 'NONE', #496, #10703, #1247, .T. ) ;
#15590 = ORIENTED_EDGE ( 'NONE', *, *, #27151, .T. ) ;
#15591 = CARTESIAN_POINT ( 'NONE',  ( 0.03008364706454716778, -0.2273032555864669124, 3.963736220472441631E-17 ) ) ;
#15592 = PLANE ( 'NONE',  #15751 ) ;
#15593 = CARTESIAN_POINT ( 'NONE',  ( 0.4763861460130703329, 0.1275996891957705826, -1.550196850393700920 ) ) ;
#15594 = AXIS2_PLACEMENT_3D ( 'NONE', #13668, #9274, #26513 ) ;
#15595 = EDGE_CURVE ( 'NONE', #16430, #21688, #24569, .T. ) ;
#15596 = CARTESIAN_POINT ( 'NONE',  ( -0.06001958459474839719, -0.4555658499976154574, -1.928289503579151187 ) ) ;
#15597 = CARTESIAN_POINT ( 'NONE',  ( 0.2564158049324918864, -0.4442166144912022552, -1.550196850393701142 ) ) ;
#15598 = CARTESIAN_POINT ( 'NONE',  ( 0.000000000000000000, 0.000000000000000000, 0.4724409448818898127 ) ) ;
#15599 = DIRECTION ( 'NONE',  ( 1.000000000000000000, 0.000000000000000000, -0.000000000000000000 ) ) ;
#15600 = AXIS2_PLACEMENT_3D ( 'NONE', #13457, #11616, #15857 ) ;
#15601 = DIRECTION ( 'NONE',  ( -1.000000000000000000, 0.000000000000000000, 0.000000000000000000 ) ) ;
#15602 = AXIS2_PLACEMENT_3D ( 'NONE', #11048, #12882, #19671 ) ;
#15603 = CYLINDRICAL_SURFACE ( 'NONE', #25055, 1.377952755905512472 ) ;
#15604 = SURFACE_STYLE_USAGE ( .BOTH. , #9785 ) ;
#15605 = CARTESIAN_POINT ( 'NONE',  ( 0.2313498293151122209, -0.4793777142568558802, 0.1322818204150990051 ) ) ;
#15606 = EDGE_CURVE ( 'NONE', #19599, #22130, #26024, .T. ) ;
#15607 = AXIS2_PLACEMENT_3D ( 'NONE', #14655, #8410, #1764 ) ;
#15608 = CARTESIAN_POINT ( 'NONE',  ( -0.07874015748238459567, 0.03414999754297557560, -0.4724409448841456749 ) ) ;
#15609 = DIRECTION ( 'NONE',  ( 0.000000000000000000, -1.000000000000000000, 0.000000000000000000 ) ) ;
#15610 = DIRECTION ( 'NONE',  ( 0.000000000000000000, 1.000000000000000000, 0.000000000000000000 ) ) ;
#15611 = ADVANCED_FACE ( 'NONE', ( #14098 ), #25495, .F. ) ;
#15612 = CIRCLE ( 'NONE', #14734, 0.5531496062992126150 ) ;
#15613 = VERTEX_POINT ( 'NONE', #10129 ) ;
#15614 = CARTESIAN_POINT ( 'NONE',  ( -0.6587140840999922142, 0.009105340598872481081, 0.2362204724409449064 ) ) ;
#15615 = VERTEX_POINT ( 'NONE', #20737 ) ;
#15616 = CARTESIAN_POINT ( 'NONE',  ( -0.3535065162672666461, -0.2712027394948650083, -1.934055118110236338 ) ) ;
#15617 = CARTESIAN_POINT ( 'NONE',  ( -0.1610509776512594748, -0.4407912692718567449, 0.1992125984251968684 ) ) ;
#15618 = CARTESIAN_POINT ( 'NONE',  ( -0.2395669291338582696, 0.000000000000000000, -0.4566929133858267376 ) ) ;
#15619 = CARTESIAN_POINT ( 'NONE',  ( -2.073220866141732523E-16, 0.07874015748031495954, 1.692913385826771533 ) ) ;
#15620 = B_SPLINE_CURVE_WITH_KNOTS ( 'NONE', 3,
 ( #15821, #5513, #15961, #9169, #13692, #17787, #24849, #13840 ),
 .UNSPECIFIED., .F., .F.,
 ( 4, 2, 2, 4 ),
 ( 0.5000000000000000000, 0.7500000000000000000, 0.8750000000000000000, 1.000000000000000000 ),
 .UNSPECIFIED. ) ;
#15621 = CARTESIAN_POINT ( 'NONE',  ( -0.4055118110236220486, -0.4724409448818898127, 0.8182917201112794858 ) ) ;
#15622 = CARTESIAN_POINT ( 'NONE',  ( 0.3740848232703748444, 0.04928467685643974500, -3.100567304031760507 ) ) ;
#15623 = CARTESIAN_POINT ( 'NONE',  ( 0.000000000000000000, 0.000000000000000000, 0.2574803149606298969 ) ) ;
#15624 = CARTESIAN_POINT ( 'NONE',  ( 0.4986013261500205074, 6.106105181202481056E-17, -0.1309055118110236116 ) ) ;
#15625 = DIRECTION ( 'NONE',  ( 0.000000000000000000, 0.9376881772560526906, 0.3474778874032439235 ) ) ;
#15626 = ADVANCED_FACE ( 'NONE', ( #14543 ), #22393, .T. ) ;
#15627 = VERTEX_POINT ( 'NONE', #6871 ) ;
#15628 = CARTESIAN_POINT ( 'NONE',  ( -0.3996230174612752095, 0.1970259548082017587, -1.934055118110236338 ) ) ;
#15629 = VECTOR ( 'NONE', #2554, 39.37007874015748143 ) ;
#15630 = VERTEX_POINT ( 'NONE', #11376 ) ;
#15631 = DIRECTION ( 'NONE',  ( 0.000000000000000000, 0.000000000000000000, 1.000000000000000000 ) ) ;
#15632 = CARTESIAN_POINT ( 'NONE',  ( -0.2577577458591218673, 0.4472135058506043759, 1.766732283464566899 ) ) ;
#15633 = CARTESIAN_POINT ( 'NONE',  ( -0.2564944395516098874, 0.4441657790107518822, 1.747047244094488194 ) ) ;
#15634 = CARTESIAN_POINT ( 'NONE',  ( 0.000000000000000000, 0.000000000000000000, -0.1740172276534823204 ) ) ;
#15635 = EDGE_LOOP ( 'NONE', ( #22565, #10660, #17402, #19244 ) ) ;
#15636 = EDGE_CURVE ( 'NONE', #6679, #21791, #12410, .T. ) ;
#15637 = PRODUCT_DEFINITION_FORMATION_WITH_SPECIFIED_SOURCE ( 'ANY', '', #27402, .NOT_KNOWN. ) ;
#15638 = CARTESIAN_POINT ( 'NONE',  ( 0.1651192144506298254, 0.3349073414798210413, -3.115157480314960647 ) ) ;
#15639 = VECTOR ( 'NONE', #2094, 39.37007874015748143 ) ;
#15640 = ORIENTED_EDGE ( 'NONE', *, *, #8190, .F. ) ;
#15641 = DIRECTION ( 'NONE',  ( -1.000000000000000000, 0.000000000000000000, 0.000000000000000000 ) ) ;
#15642 = CARTESIAN_POINT ( 'NONE',  ( 0.4716287720755726887, -0.1069935333116613374, 0.2008762816168113419 ) ) ;
#15643 = ADVANCED_FACE ( 'NONE', ( #26417 ), #23834, .T. ) ;
#15644 = CARTESIAN_POINT ( 'NONE',  ( -0.2041304421298503480, 0.2660793235464394280, 1.953740157480315043 ) ) ;
#15645 = ORIENTED_EDGE ( 'NONE', *, *, #6822, .T. ) ;
#15646 = ORIENTED_EDGE ( 'NONE', *, *, #14066, .T. ) ;
#15647 = AXIS2_PLACEMENT_3D ( 'NONE', #13932, #25725, #7289 ) ;
#15648 = EDGE_CURVE ( 'NONE', #13218, #2702, #18957, .T. ) ;
#15649 = CARTESIAN_POINT ( 'NONE',  ( 0.4446020952038907681, 5.549066237130534971E-17, -1.934055118110236338 ) ) ;
#15650 = ORIENTED_EDGE ( 'NONE', *, *, #10391, .T. ) ;
#15651 = VERTEX_POINT ( 'NONE', #7638 ) ;
#15652 = ORIENTED_EDGE ( 'NONE', *, *, #19588, .F. ) ;
#15653 = DIRECTION ( 'NONE',  ( 0.000000000000000000, 1.000000000000000000, -1.224646799147353207E-16 ) ) ;
#15654 = ITEM_DEFINED_TRANSFORMATION ( 'NONE', 'NONE', #16098,  #11588 ) ;
#15655 = CARTESIAN_POINT ( 'NONE',  ( 0.6995334740348704283, 0.7637040338457791178, -0.01440115984997634123 ) ) ;
#15656 = EDGE_LOOP ( 'NONE', ( #14462, #5814, #27842, #5155 ) ) ;
#15657 = CARTESIAN_POINT ( 'NONE',  ( 0.000000000000000000, 0.000000000000000000, 1.953740157480315043 ) ) ;
#15658 = CARTESIAN_POINT ( 'NONE',  ( 0.2817310484609195642, 0.2161381151962948888, 1.953740157480315043 ) ) ;
#15659 = CARTESIAN_POINT ( 'NONE',  ( 0.7874015748031496509, -5.862181872755905604E-06, -1.869015748010449007 ) ) ;
#15660 = ADVANCED_FACE ( 'NONE', ( #11447 ), #24434, .F. ) ;
#15661 = CIRCLE ( 'NONE', #26464, 1.988188976307287970 ) ;
#15662 = CARTESIAN_POINT ( 'NONE',  ( -0.2362204724409449064, -0.4724409448818898127, -0.6874452634183682020 ) ) ;
#15663 = DIRECTION ( 'NONE',  ( -1.000000000000000000, 0.000000000000000000, 0.000000000000000000 ) ) ;
#15664 = CARTESIAN_POINT ( 'NONE',  ( 0.3149606299212598381, 0.000000000000000000, -3.666338582670846780 ) ) ;
#15665 = FACE_OUTER_BOUND ( 'NONE', #17920, .T. ) ;
#15666 = CARTESIAN_POINT ( 'NONE',  ( 0.1181102362204724532, 1.446433227339393765E-17, 0.6299212598425196763 ) ) ;
#15667 = EDGE_LOOP ( 'NONE', ( #16679, #18810, #24723, #7185 ) ) ;
#15668 = EDGE_CURVE ( 'NONE', #16023, #25509, #8362, .T. ) ;
#15669 = CARTESIAN_POINT ( 'NONE',  ( 0.3751294191746885609, 0.2999672986753447734, 0.2362204724409446843 ) ) ;
#15670 = ( NAMED_UNIT ( * ) SI_UNIT ( $, .STERADIAN. ) SOLID_ANGLE_UNIT ( ) ) ;
#15671 = VERTEX_POINT ( 'NONE', #15017 ) ;
#15672 = CARTESIAN_POINT ( 'NONE',  ( 0.1522836969735573143, -0.4909267390297480382, 0.05591742528025181458 ) ) ;
#15673 = EDGE_LOOP ( 'NONE', ( #17975, #14319, #23958, #26617 ) ) ;
#15674 = CARTESIAN_POINT ( 'NONE',  ( -4.821444091131312140E-17, -0.3937007874015748254, 0.3425196850393700809 ) ) ;
#15675 = TOROIDAL_SURFACE ( 'NONE', #367, 0.3070866141732283561, 0.01181102362204724393 ) ;
#15676 = ORIENTED_EDGE ( 'NONE', *, *, #7937, .T. ) ;
#15677 = CARTESIAN_POINT ( 'NONE',  ( 0.5511811023622048555, 0.03607471876262481614, 0.9399606299212598381 ) ) ;
#15678 = ORIENTED_EDGE ( 'NONE', *, *, #6471, .F. ) ;
#15679 = DIRECTION ( 'NONE',  ( -1.000000000000000000, 0.000000000000000000, 0.000000000000000000 ) ) ;
#15680 = CARTESIAN_POINT ( 'NONE',  ( 0.1189624676717044721, -0.3253923344978163490, 0.1276989850526606129 ) ) ;
#15681 = CARTESIAN_POINT ( 'NONE',  ( 0.1493295869868994930, 0.4796200322303180164, -0.01881014177756113945 ) ) ;
#15682 = DIRECTION ( 'NONE',  ( 1.000000000000000000, 0.000000000000000000, 0.000000000000000000 ) ) ;
#15683 = DIRECTION ( 'NONE',  ( 0.000000000000000000, -1.000000000000000000, 0.000000000000000000 ) ) ;
#15684 = DIRECTION ( 'NONE',  ( 0.000000000000000000, -1.000000000000000000, 0.000000000000000000 ) ) ;
#15685 = CARTESIAN_POINT ( 'NONE',  ( 0.02919171328787628986, 0.07406745870972507306, -0.4660331883676341880 ) ) ;
#15686 = CARTESIAN_POINT ( 'NONE',  ( 0.3543307086614173040, -1.934043700787401319E-18, 0.000000000000000000 ) ) ;
#15687 = CARTESIAN_POINT ( 'NONE',  ( -0.3346456692913385988, 0.02190250779246044610, 1.953740157480315043 ) ) ;
#15688 = EDGE_CURVE ( 'NONE', #5827, #24512, #1571, .T. ) ;
#15689 = AXIS2_PLACEMENT_3D ( 'NONE', #4683, #19398, #2430 ) ;
#15690 = FACE_OUTER_BOUND ( 'NONE', #1475, .T. ) ;
#15691 = EDGE_CURVE ( 'NONE', #7980, #27336, #13553, .T. ) ;
#15692 = CARTESIAN_POINT ( 'NONE',  ( 0.4063220079890811354, -0.2348123150948578930, 0.07637549214372854611 ) ) ;
#15693 = CARTESIAN_POINT ( 'NONE',  ( 0.07472527936311225416, 0.5671862884095085766, 0.9399606299212598381 ) ) ;
#15694 = CARTESIAN_POINT ( 'NONE',  ( -0.06699590632655402778, -0.5118110236220471121, 1.766732283464566899 ) ) ;
#15695 = ( GEOMETRIC_REPRESENTATION_CONTEXT ( 3 ) GLOBAL_UNCERTAINTY_ASSIGNED_CONTEXT ( ( #10501 ) ) GLOBAL_UNIT_ASSIGNED_CONTEXT ( ( #23442, #21307, #25543 ) ) REPRESENTATION_CONTEXT ( 'NONE', 'WORKASPACE' ) ) ;
#15696 = AXIS2_PLACEMENT_3D ( 'NONE', #5133, #1060, #2863 ) ;
#15697 = DIRECTION ( 'NONE',  ( 1.000000000000000000, 0.000000000000000000, 0.000000000000000000 ) ) ;
#15698 = DIRECTION ( 'NONE',  ( 0.000000000000000000, 0.000000000000000000, -1.000000000000000000 ) ) ;
#15699 = EDGE_CURVE ( 'NONE', #21158, #247, #5236, .T. ) ;
#15700 = CARTESIAN_POINT ( 'NONE',  ( -0.4834654033798361228, -0.1110087727118397871, 0.1734435147621542217 ) ) ;
#15701 = ORIENTED_EDGE ( 'NONE', *, *, #3170, .T. ) ;
#15702 = EDGE_CURVE ( 'NONE', #27117, #4298, #2111, .T. ) ;
#15703 = DIRECTION ( 'NONE',  ( 0.000000000000000000, 0.000000000000000000, -1.000000000000000000 ) ) ;
#15704 = FACE_OUTER_BOUND ( 'NONE', #13963, .T. ) ;
#15705 = ORIENTED_EDGE ( 'NONE', *, *, #14778, .T. ) ;
#15706 = DIRECTION ( 'NONE',  ( 0.000000000000000000, -1.000000000000000000, 0.000000000000000000 ) ) ;
#15707 = EDGE_LOOP ( 'NONE', ( #27548, #1091 ) ) ;
#15708 = TOROIDAL_SURFACE ( 'NONE', #16154, 0.4848217985909654137, 0.01377952755905511792 ) ;
#15709 = ( CONVERSION_BASED_UNIT ( 'INCH', #7094 ) LENGTH_UNIT ( ) NAMED_UNIT ( #20779 ) ) ;
#15710 = AXIS2_PLACEMENT_3D ( 'NONE', #16849, #16413, #25458 ) ;
#15711 = AXIS2_PLACEMENT_3D ( 'NONE', #6830, #11333, #8936 ) ;
#15712 = CARTESIAN_POINT ( 'NONE',  ( -0.1968503937007874127, 0.07874015748031495954, -0.04546065111729338803 ) ) ;
#15713 = CARTESIAN_POINT ( 'NONE',  ( 0.7873253891977465280, 0.2512985515673845649, -0.2758449551032512992 ) ) ;
#15714 = CARTESIAN_POINT ( 'NONE',  ( -0.07870736637777375755, 0.2165354330708661457, -3.608715228343988279 ) ) ;
#15715 = CARTESIAN_POINT ( 'NONE',  ( 0.6119360453657027854, 0.1072290460172409393, 0.2574803149606298969 ) ) ;
#15716 = ORIENTED_EDGE ( 'NONE', *, *, #16578, .F. ) ;
#15717 = AXIS2_PLACEMENT_3D ( 'NONE', #6103, #6505, #10589 ) ;
#15718 = DIRECTION ( 'NONE',  ( 1.000000000000000000, 0.000000000000000000, 0.000000000000000000 ) ) ;
#15719 = EDGE_CURVE ( 'NONE', #9665, #3782, #265, .T. ) ;
#15720 = CARTESIAN_POINT ( 'NONE',  ( 0.2796934465393767222, -0.3645739570812915331, -1.928289503579138753 ) ) ;
#15721 = CARTESIAN_POINT ( 'NONE',  ( 0.3149606299212598381, -0.3346456692913385988, 4.098227477461615257E-17 ) ) ;
#15722 = CARTESIAN_POINT ( 'NONE',  ( 0.0005189969344232283309, 0.3771649972486724733, 0.1992125984251968684 ) ) ;
#15723 = ADVANCED_FACE ( 'NONE', ( #14442 ), #9899, .T. ) ;
#15724 = CARTESIAN_POINT ( 'NONE',  ( -0.1771653543307086520, 0.5570866141732283561, 0.000000000000000000 ) ) ;
#15725 = CARTESIAN_POINT ( 'NONE',  ( -0.4930758245789425009, 0.08754571829529331217, 0.2574803149606298969 ) ) ;
#15726 = ADVANCED_BREP_SHAPE_REPRESENTATION ( 'Cam Shaft', ( #12711, #11588 ), #2999 ) ;
#15727 = EDGE_CURVE ( 'NONE', #8482, #2317, #2414, .T. ) ;
#15728 = AXIS2_PLACEMENT_3D ( 'NONE', #5608, #24805, #10116 ) ;
#15729 = AXIS2_PLACEMENT_3D ( 'NONE', #26507, #820, #9409 ) ;
#15730 = EDGE_CURVE ( 'NONE', #27302, #16370, #11509, .T. ) ;
#15731 = AXIS2_PLACEMENT_3D ( 'NONE', #2296, #13444, #358 ) ;
#15732 = CARTESIAN_POINT ( 'NONE',  ( -0.6165893942483189338, -0.1247741027201273722, 0.07187346404476555040 ) ) ;
#15733 = DIRECTION ( 'NONE',  ( 0.000000000000000000, 0.000000000000000000, 1.000000000000000000 ) ) ;
#15734 = CARTESIAN_POINT ( 'NONE',  ( 0.000000000000000000, 0.000000000000000000, -0.01377952755905511792 ) ) ;
#15735 = CARTESIAN_POINT ( 'NONE',  ( 0.4078284417489183022, 0.4849914877866832175, 0.2481708550941282843 ) ) ;
#15736 = CARTESIAN_POINT ( 'NONE',  ( -0.0006681923949012172652, 0.6336721034116280515, 0.2481708550951330083 ) ) ;
#15737 = EDGE_CURVE ( 'NONE', #23039, #10528, #20972, .T. ) ;
#15739 = FACE_OUTER_BOUND ( 'NONE', #19180, .T. ) ;
#15738 = CIRCLE ( 'NONE', #15323, 0.4786070381542913421 ) ;
#15740 = DIRECTION ( 'NONE',  ( 0.000000000000000000, 0.000000000000000000, 1.000000000000000000 ) ) ;
#15741 = ORIENTED_EDGE ( 'NONE', *, *, #17788, .T. ) ;
#15742 = CARTESIAN_POINT ( 'NONE',  ( 0.3543307086614174151, 0.02327295973586337649, 1.953740157480314821 ) ) ;
#15743 = EDGE_CURVE ( 'NONE', #3368, #4856, #24719, .T. ) ;
#15744 = VERTEX_POINT ( 'NONE', #8574 ) ;
#15745 = CARTESIAN_POINT ( 'NONE',  ( 0.4498374011143674855, 0.05926487674658936083, -1.934055118110236338 ) ) ;
#15746 = CARTESIAN_POINT ( 'NONE',  ( -0.4067073728345488304, -0.2341441294389850492, 0.07637795275590551769 ) ) ;
#15747 = CARTESIAN_POINT ( 'NONE',  ( -0.03532354024591775193, -0.6299212598425196763, -0.5531496062992126150 ) ) ;
#15748 = CARTESIAN_POINT ( 'NONE',  ( -0.5112608635011182123, 0.5325127325997165428, 0.1663800295771515891 ) ) ;
#15749 = CIRCLE ( 'NONE', #2647, 0.3070866141732283561 ) ;
#15750 = FACE_OUTER_BOUND ( 'NONE', #1416, .T. ) ;
#15751 = AXIS2_PLACEMENT_3D ( 'NONE', #22068, #11064, #19689 ) ;
#15752 = CARTESIAN_POINT ( 'NONE',  ( -0.2104048168850177758, -0.4354435989233408355, 0.2008762816475422042 ) ) ;
#15753 = CARTESIAN_POINT ( 'NONE',  ( 0.2296683860596781812, -0.2993674444872274631, -3.100567304031764060 ) ) ;
#15754 = ( REPRESENTATION_RELATIONSHIP ('NONE','NONE', #12434, #16232 ) REPRESENTATION_RELATIONSHIP_WITH_TRANSFORMATION ( #24692 )SHAPE_REPRESENTATION_RELATIONSHIP( ) ) ;
#15755 = AXIS2_PLACEMENT_3D ( 'NONE', #11544, #13957, #2915 ) ;
#15756 = CARTESIAN_POINT ( 'NONE',  ( 1.446433227339387294E-17, 0.07874015748031495954, -1.574803149606299524 ) ) ;
#15757 = ORIENTED_EDGE ( 'NONE', *, *, #20658, .F. ) ;
#15758 = DIRECTION ( 'NONE',  ( -0.3420201433256691015, -0.9396926207859082059, 0.000000000000000000 ) ) ;
#15759 = EDGE_CURVE ( 'NONE', #13737, #11023, #21572, .T. ) ;
#15760 = B_SPLINE_CURVE_WITH_KNOTS ( 'NONE', 3,
 ( #21787, #11051, #8921, #6818, #17548, #26162 ),
 .UNSPECIFIED., .F., .F.,
 ( 4, 2, 4 ),
 ( 0.5000000000000000000, 0.7500000000000000000, 1.000000000000000000 ),
 .UNSPECIFIED. ) ;
#15761 = AXIS2_PLACEMENT_3D ( 'NONE', #4145, #19253, #12478 ) ;
#15762 = ADVANCED_FACE ( 'NONE', ( #9521 ), #20314, .F. ) ;
#15763 = SHAPE_DEFINITION_REPRESENTATION ( #8681, #15008 ) ;
#15764 = EDGE_LOOP ( 'NONE', ( #8984, #12267, #24586, #21167 ) ) ;
#15765 = CARTESIAN_POINT ( 'NONE',  ( 0.3777066424217488949, 0.3020248451665031308, 0.2715646632922476544 ) ) ;
#15766 = DIRECTION ( 'NONE',  ( -0.9790454724845842893, 0.2036417511401760472, 0.000000000000000000 ) ) ;
#15767 = CARTESIAN_POINT ( 'NONE',  ( 0.2564944395515434961, -0.4441657790107952364, 1.766732283464566899 ) ) ;
#15768 = ( CONVERSION_BASED_UNIT ( 'INCH', #5012 ) LENGTH_UNIT ( ) NAMED_UNIT ( #3625 ) ) ;
#15769 = CONICAL_SURFACE ( 'NONE', #11705, 0.04546065111729338803, 1.047197549999998811 ) ;
#15770 = CARTESIAN_POINT ( 'NONE',  ( -0.3702005978258584573, -0.04877294052295926691, -3.115157480314960647 ) ) ;
#15771 = ORIENTED_EDGE ( 'NONE', *, *, #18379, .T. ) ;
#15772 = DIRECTION ( 'NONE',  ( -1.000000000000000000, 0.000000000000000000, 0.000000000000000000 ) ) ;
#15773 = CIRCLE ( 'NONE', #21186, 0.1181010187939084827 ) ;
#15774 = FACE_OUTER_BOUND ( 'NONE', #3913, .T. ) ;
#15775 = CARTESIAN_POINT ( 'NONE',  ( 0.2521176338356516666, -0.2211428102655709216, 1.953740157480315043 ) ) ;
#15776 = ORIENTED_EDGE ( 'NONE', *, *, #8388, .F. ) ;
#15777 = ORIENTED_EDGE ( 'NONE', *, *, #15822, .F. ) ;
#15778 = ORIENTED_EDGE ( 'NONE', *, *, #665, .F. ) ;
#15779 = DIRECTION ( 'NONE',  ( 0.000000000000000000, 1.000000000000000000, 0.000000000000000000 ) ) ;
#15780 = VERTEX_POINT ( 'NONE', #18600 ) ;
#15781 = ORIENTED_EDGE ( 'NONE', *, *, #23960, .T. ) ;
#15782 = FACE_OUTER_BOUND ( 'NONE', #16681, .T. ) ;
#15783 = CARTESIAN_POINT ( 'NONE',  ( -0.2490711204941342405, 0.9131938423895413770, -0.7142170566240019225 ) ) ;
#15784 = CARTESIAN_POINT ( 'NONE',  ( -0.4173228346456693272, 5.110730736599190647E-17, 0.4488188976377953110 ) ) ;
#15785 = DIRECTION ( 'NONE',  ( 0.000000000000000000, 0.000000000000000000, -1.000000000000000000 ) ) ;
#15786 = AXIS2_PLACEMENT_3D ( 'NONE', #6144, #8247, #25759 ) ;
#15787 = CIRCLE ( 'NONE', #27088, 0.1771653543307086520 ) ;
#15788 = CARTESIAN_POINT ( 'NONE',  ( 0.000000000000000000, 0.000000000000000000, 0.7844728274238290666 ) ) ;
#15789 = DIRECTION ( 'NONE',  ( 1.000000000000000000, 0.000000000000000000, 0.000000000000000000 ) ) ;
#15790 = CARTESIAN_POINT ( 'NONE',  ( 0.2817310484609266696, -0.2161381151962942504, 1.953740157480315043 ) ) ;
#15791 = EDGE_CURVE ( 'NONE', #7018, #5696, #13286, .T. ) ;
#15792 = CARTESIAN_POINT ( 'NONE',  ( -0.5378064472800889728, -0.3110113600220764107, 0.2574819594177527593 ) ) ;
#15793 = CARTESIAN_POINT ( 'NONE',  ( -0.2311492806687369950, -0.4794744477484330636, 0.1322810039474933141 ) ) ;
#15794 = CARTESIAN_POINT ( 'NONE',  ( -0.02919171328787628986, -0.07406745870972507306, -0.4660331883676341880 ) ) ;
#15795 = CARTESIAN_POINT ( 'NONE',  ( -0.3765118517642104257, 2.305470170520414967E-17, -3.100567304031763172 ) ) ;
#15796 = CARTESIAN_POINT ( 'NONE',  ( 0.5085118447801502128, -0.06699507805371243685, 1.747047244094488194 ) ) ;
#15797 = VERTEX_POINT ( 'NONE', #146 ) ;
#15798 = ORIENTED_EDGE ( 'NONE', *, *, #17839, .T. ) ;
#15799 = CARTESIAN_POINT ( 'NONE',  ( 0.000000000000000000, 0.6102362204724409711, -1.156053543307086666E-17 ) ) ;
#15800 = ORIENTED_EDGE ( 'NONE', *, *, #18641, .T. ) ;
#15801 = DIRECTION ( 'NONE',  ( 0.000000000000000000, -1.000000000000000000, 0.000000000000000000 ) ) ;
#15802 = ORIENTED_EDGE ( 'NONE', *, *, #9003, .F. ) ;
#15803 = CARTESIAN_POINT ( 'NONE',  ( -0.4067073728345488304, -0.2341441294389850492, 0.07637795275590551769 ) ) ;
#15804 = CONICAL_SURFACE ( 'NONE', #7223, 1.112204724409448842, 0.7853981624999977207 ) ;
#15805 = CARTESIAN_POINT ( 'NONE',  ( 0.03220957031753989008, 0.4921259842519685179, -1.569881889763779625 ) ) ;
#15806 = CARTESIAN_POINT ( 'NONE',  ( 0.6864238947233102239, -0.1574599019769754027, 0.1443310008636487507 ) ) ;
#15807 = ORIENTED_EDGE ( 'NONE', *, *, #19632, .T. ) ;
#15808 = CARTESIAN_POINT ( 'NONE',  ( 0.5526079293737398146, 0.1480156394741914405, 0.9399606299212598381 ) ) ;
#15809 = ORIENTED_EDGE ( 'NONE', *, *, #7082, .F. ) ;
#15810 = CARTESIAN_POINT ( 'NONE',  ( 0.000000000000000000, 0.000000000000000000, -0.05856299212598425896 ) ) ;
#15811 = DIRECTION ( 'NONE',  ( 0.000000000000000000, 0.000000000000000000, 1.000000000000000000 ) ) ;
#15812 = CIRCLE ( 'NONE', #19427, 0.3346456692913385988 ) ;
#15813 = CARTESIAN_POINT ( 'NONE',  ( 0.1196556571320694373, -0.3272932875280350484, 0.1166443193822704893 ) ) ;
#15814 = ITEM_DEFINED_TRANSFORMATION ( 'NONE', 'NONE', #25617,  #11588 ) ;
#15815 = DIRECTION ( 'NONE',  ( 0.000000000000000000, -1.000000000000000000, 0.000000000000000000 ) ) ;
#15816 = CARTESIAN_POINT ( 'NONE',  ( -2.183966630091013010E-17, 0.6212598425196852459, 0.09684793308443542803 ) ) ;
#15817 = DIRECTION ( 'NONE',  ( 1.000000000000000000, 0.000000000000000000, 0.000000000000000000 ) ) ;
#15818 = DIRECTION ( 'NONE',  ( 0.000000000000000000, 0.000000000000000000, 1.000000000000000000 ) ) ;
#15819 = FACE_BOUND ( 'NONE', #3436, .T. ) ;
#15820 = CARTESIAN_POINT ( 'NONE',  ( -0.3777066424189819971, 0.3020248451642900678, 0.2715646632795538085 ) ) ;
#15821 = CARTESIAN_POINT ( 'NONE',  ( 0.4681308612729627727, -0.1074986424507606286, 0.2362204724409450174 ) ) ;
#15822 = EDGE_CURVE ( 'NONE', #24679, #27463, #7433, .T. ) ;
#15823 = CARTESIAN_POINT ( 'NONE',  ( 0.000000000000000000, 0.000000000000000000, -0.2755905511811023723 ) ) ;
#15824 = CIRCLE ( 'NONE', #14496, 0.3771653543307086909 ) ;
#15825 = CARTESIAN_POINT ( 'NONE',  ( -0.6266852695743893031, -0.1062821802600274479, 0.2318330448317133807 ) ) ;
#15826 = CARTESIAN_POINT ( 'NONE',  ( 0.4126915023386704684, -0.2375990494935494579, 0.1212655228829027515 ) ) ;
#15827 = CARTESIAN_POINT ( 'NONE',  ( -0.1294857240059045234, -0.3542416573274181357, 0.07637795275590551769 ) ) ;
#15828 = CARTESIAN_POINT ( 'NONE',  ( 0.000000000000000000, 0.000000000000000000, -0.4566929133858267376 ) ) ;
#15829 = CIRCLE ( 'NONE', #18067, 0.1318897637674583401 ) ;
#15830 = ORIENTED_EDGE ( 'NONE', *, *, #8188, .F. ) ;
#15831 = DIRECTION ( 'NONE',  ( 0.000000000000000000, 0.000000000000000000, -1.000000000000000000 ) ) ;
#15832 = DIRECTION ( 'NONE',  ( 1.000000000000000000, 0.000000000000000000, 0.000000000000000000 ) ) ;
#15833 = CARTESIAN_POINT ( 'NONE',  ( -0.07669076177803985095, 0.1968503937007873850, -3.568838416488017362 ) ) ;
#15834 = ORIENTED_EDGE ( 'NONE', *, *, #25396, .F. ) ;
#15835 = CARTESIAN_POINT ( 'NONE',  ( 0.000000000000000000, 0.000000000000000000, -0.01377952755905511792 ) ) ;
#15836 = VERTEX_POINT ( 'NONE', #11245 ) ;
#15837 = EDGE_CURVE ( 'NONE', #10141, #25275, #11233, .T. ) ;
#15838 = CARTESIAN_POINT ( 'NONE',  ( 0.4339912984563291110, -0.2498791196563492356, 0.2574803149606298969 ) ) ;
#15839 = AXIS2_PLACEMENT_3D ( 'NONE', #17966, #24766, #7256 ) ;
#15840 = CARTESIAN_POINT ( 'NONE',  ( 0.7845931698711713365, 0.5239360887457676919, 0.1316939677558954802 ) ) ;
#15841 = CARTESIAN_POINT ( 'NONE',  ( -0.5118110236220473341, 0.000000000000000000, -1.550196850393700920 ) ) ;
#15842 = ( GEOMETRIC_REPRESENTATION_CONTEXT ( 3 ) GLOBAL_UNCERTAINTY_ASSIGNED_CONTEXT ( ( #7911 ) ) GLOBAL_UNIT_ASSIGNED_CONTEXT ( ( #15768, #18418, #3303 ) ) REPRESENTATION_CONTEXT ( 'NONE', 'WORKASPACE' ) ) ;
#15843 = TOROIDAL_SURFACE ( 'NONE', #3661, 0.6102362204724409711, 0.1299212598425196763 ) ;
#15844 = CARTESIAN_POINT ( 'NONE',  ( 0.000000000000000000, 0.000000000000000000, 0.2362204724409449064 ) ) ;
#15845 = EDGE_CURVE ( 'NONE', #25529, #18018, #1727, .T. ) ;
#15846 = EDGE_LOOP ( 'NONE', ( #13971, #4554, #20002 ) ) ;
#15847 = CARTESIAN_POINT ( 'NONE',  ( 0.1677079028045456166, 0.2904160862623617056, 1.973425196850393970 ) ) ;
#15848 = CARTESIAN_POINT ( 'NONE',  ( 0.03349795313024148125, 0.5118110236220473341, -1.550196850393700920 ) ) ;
#15849 = CARTESIAN_POINT ( 'NONE',  ( -0.2031943647053863211, 0.4121342552748505916, -1.928289503579144748 ) ) ;
#15850 = CARTESIAN_POINT ( 'NONE',  ( 0.0004986409324247901122, 0.3484797321232478429, 0.1589462317930195046 ) ) ;
#15851 = DIRECTION ( 'NONE',  ( 0.000000000000000000, 1.000000000000000000, 0.000000000000000000 ) ) ;
#15852 = CARTESIAN_POINT ( 'NONE',  ( 0.3082037322261920176, 0.3663931537946265582, 0.08349695147694113917 ) ) ;
#15853 = CARTESIAN_POINT ( 'NONE',  ( 0.3001918266902277588, 0.3912931228432131592, -1.569881889763779625 ) ) ;
#15854 = CARTESIAN_POINT ( 'NONE',  ( 8.741913385826771462E-17, -0.1673228346456692994, 2.049113738730807629E-17 ) ) ;
#15855 = CIRCLE ( 'NONE', #5962, 0.1181102362204720091 ) ;
#15856 = CARTESIAN_POINT ( 'NONE',  ( 0.2705157149885996093, 0.000000000000000000, 0.000000000000000000 ) ) ;
#15857 = DIRECTION ( 'NONE',  ( 0.000000000000000000, 1.000000000000000000, 0.000000000000000000 ) ) ;
#15858 = ( NAMED_UNIT ( * ) PLANE_ANGLE_UNIT ( ) SI_UNIT ( $, .RADIAN. ) ) ;
#15859 = CARTESIAN_POINT ( 'NONE',  ( 0.4233199042360576425, 0.5034331896086758906, 0.1461456498285838845 ) ) ;
#15860 = ORIENTED_EDGE ( 'NONE', *, *, #6809, .F. ) ;
#15861 = CIRCLE ( 'NONE', #14976, 0.3937007874015748254 ) ;
#15862 = EDGE_CURVE ( 'NONE', #18324, #3673, #25963, .T. ) ;
#15863 = DIRECTION ( 'NONE',  ( 0.1736481776669299981, -0.9848077530122081313, 0.000000000000000000 ) ) ;
#15864 = CARTESIAN_POINT ( 'NONE',  ( 0.1755067523729419432, 0.3028750839302637998, 0.5245950337139047015 ) ) ;
#15865 = ORIENTED_EDGE ( 'NONE', *, *, #18612, .F. ) ;
#15866 = CARTESIAN_POINT ( 'NONE',  ( 0.3362580771780208644, 0.1141156591735774661, 1.953740157480315043 ) ) ;
#15867 = ORIENTED_EDGE ( 'NONE', *, *, #825, .F. ) ;
#15868 = VERTEX_POINT ( 'NONE', #22927 ) ;
#15869 = CARTESIAN_POINT ( 'NONE',  ( -0.05926487674658171417, -0.4498374011143209117, -1.934055118110236338 ) ) ;
#15870 = DIRECTION ( 'NONE',  ( -1.000000000000000000, 0.000000000000000000, 0.000000000000000000 ) ) ;
#15871 = DIRECTION ( 'NONE',  ( 1.000000000000000000, 0.000000000000000000, 0.000000000000000000 ) ) ;
#15872 = CARTESIAN_POINT ( 'NONE',  ( 0.09777739100673171757, 0.2994019835985785583, -3.259649345945281329 ) ) ;
#15873 = EDGE_CURVE ( 'NONE', #5084, #16925, #22379, .T. ) ;
#15874 = EDGE_CURVE ( 'NONE', #12620, #10641, #11346, .T. ) ;
#15875 = ORIENTED_EDGE ( 'NONE', *, *, #8806, .T. ) ;
#15876 = DIRECTION ( 'NONE',  ( -0.2036417511401759084, 0.4895227362422917006, -0.8478782506317888989 ) ) ;
#15877 = DIRECTION ( 'NONE',  ( -0.000000000000000000, -1.000000000000000000, -0.000000000000000000 ) ) ;
#15878 = EDGE_CURVE ( 'NONE', #3924, #8098, #10618, .T. ) ;
#15879 = CARTESIAN_POINT ( 'NONE',  ( 0.5905511811023621549, 0.000000000000000000, 0.000000000000000000 ) ) ;
#15880 = CARTESIAN_POINT ( 'NONE',  ( -0.3937007873768824662, 4.821444090828918336E-17, 2.090519358671640647E-11 ) ) ;
#15881 = CIRCLE ( 'NONE', #21301, 0.3937007874015748254 ) ;
#15882 = CARTESIAN_POINT ( 'NONE',  ( 0.3905379133858267737, 0.2805118110236220486, 0.4858607088160724063 ) ) ;
#15883 = CARTESIAN_POINT ( 'NONE',  ( 0.1668516812751341394, -0.3384212623783144913, -3.100567304031760951 ) ) ;
#15884 = EDGE_CURVE ( 'NONE', #26909, #19062, #14030, .T. ) ;
#15885 = CARTESIAN_POINT ( 'NONE',  ( 0.0003954787107570253350, 0.5007872847596378518, 0.09684874903502814492 ) ) ;
#15886 = ORIENTED_EDGE ( 'NONE', *, *, #5062, .F. ) ;
#15887 = CARTESIAN_POINT ( 'NONE',  ( -0.2712027394948746117, 0.3535065162672773043, -1.934055118110236338 ) ) ;
#15888 = AXIS2_PLACEMENT_3D ( 'NONE', #6225, #18438, #16622 ) ;
#15889 = CARTESIAN_POINT ( 'NONE',  ( -2.184900367198595585E-17, 0.6212598425196850238, 0.2574827755769818483 ) ) ;
#15890 = ORIENTED_EDGE ( 'NONE', *, *, #26245, .T. ) ;
#15891 = ORIENTED_EDGE ( 'NONE', *, *, #20124, .F. ) ;
#15892 = VERTEX_POINT ( 'NONE', #22361 ) ;
#15893 = CARTESIAN_POINT ( 'NONE',  ( -0.3338887748335567229, -1.104088614729972440, -0.7990416445823268488 ) ) ;
#15894 = LINE ( 'NONE', #17856, #9066 ) ;
#15895 = CARTESIAN_POINT ( 'NONE',  ( -0.4441657790107816917, 0.2564944395515652564, 1.747047244094488194 ) ) ;
#15896 = SPHERICAL_SURFACE ( 'NONE', #2572, 0.1299232283464566984 ) ;
#15897 = ORIENTED_EDGE ( 'NONE', *, *, #10391, .F. ) ;
#15898 = CONICAL_SURFACE ( 'NONE', #24015, 0.08582677165393072516, 0.7853981625000011624 ) ;
#15899 = CARTESIAN_POINT ( 'NONE',  ( -0.2993674444872340690, 0.2296683860596682170, -3.100567304031764060 ) ) ;
#15900 = ORIENTED_EDGE ( 'NONE', *, *, #27381, .F. ) ;
#15901 = CARTESIAN_POINT ( 'NONE',  ( 0.6202606299212598540, -6.779653543307085645E-20, 0.000000000000000000 ) ) ;
#15902 = CARTESIAN_POINT ( 'NONE',  ( -0.5905511811023621549, 1.131889763779527547, 0.000000000000000000 ) ) ;
#15903 = ORIENTED_EDGE ( 'NONE', *, *, #7913, .F. ) ;
#15904 = ORIENTED_EDGE ( 'NONE', *, *, #24635, .F. ) ;
#15905 = VERTEX_POINT ( 'NONE', #2985 ) ;
#15906 = EDGE_CURVE ( 'NONE', #8482, #17618, #6130, .T. ) ;
#15907 = CARTESIAN_POINT ( 'NONE',  ( 0.1286734528930086607, -0.3545375539099149265, 0.1992142436757342316 ) ) ;
#15908 = EDGE_LOOP ( 'NONE', ( #11880, #10558, #21063, #289 ) ) ;
#15909 = DIRECTION ( 'NONE',  ( 0.000000000000000000, 0.000000000000000000, -1.000000000000000000 ) ) ;
#15910 = ORIENTED_EDGE ( 'NONE', *, *, #12178, .F. ) ;
#15911 = ORIENTED_EDGE ( 'NONE', *, *, #12607, .T. ) ;
#15912 = FACE_OUTER_BOUND ( 'NONE', #6105, .T. ) ;
#15913 = CARTESIAN_POINT ( 'NONE',  ( -0.02063524494269025969, 0.1968503937007874127, -3.624905640648360183 ) ) ;
#15914 = EDGE_CURVE ( 'NONE', #4492, #3371, #10929, .T. ) ;
#15915 = CARTESIAN_POINT ( 'NONE',  ( 0.2083728861314909642, 0.3778799683983641300, -0.2992345713071495883 ) ) ;
#15916 = CARTESIAN_POINT ( 'NONE',  ( 0.04840761057748826229, 0.1968503937007874127, -3.209693978926679847 ) ) ;
#15917 = CARTESIAN_POINT ( 'NONE',  ( 0.4895462770359960136, 1.042587244177305195, -0.2949132003431571003 ) ) ;
#15918 = PRODUCT_DEFINITION_SHAPE ( 'NONE', 'NONE',  #27897 ) ;
#15919 = CIRCLE ( 'NONE', #20887, 0.1318897637674579792 ) ;
#15920 = CIRCLE ( 'NONE', #6453, 0.1299232283464566706 ) ;
#15921 = VERTEX_POINT ( 'NONE', #20239 ) ;
#15922 = CARTESIAN_POINT ( 'NONE',  ( 0.06048688188729473697, 0.2165354330708661734, -3.193930428897816753 ) ) ;
#15923 = CARTESIAN_POINT ( 'NONE',  ( -0.2924088307484721816, -0.1685339107540411718, 1.973425196850393526 ) ) ;
#15924 = CARTESIAN_POINT ( 'NONE',  ( -0.09187177619658792871, 0.3429980251342187314, 1.953740157480315043 ) ) ;
#15925 = EDGE_CURVE ( 'NONE', #13999, #11422, #26405, .T. ) ;
#15926 = CARTESIAN_POINT ( 'NONE',  ( -0.09842519685039370636, 0.2991866959364303247, -3.272637795275590733 ) ) ;
#15927 = AXIS2_PLACEMENT_3D ( 'NONE', #18337, #997, #14131 ) ;
#15928 = CARTESIAN_POINT ( 'NONE',  ( 0.1522836969735573143, 0.1970374587079574968, -0.4531137400369417145 ) ) ;
#15929 = CARTESIAN_POINT ( 'NONE',  ( -0.09842519685039370636, -0.07874015748031495954, -0.04546065111729338803 ) ) ;
#15930 = DIRECTION ( 'NONE',  ( 0.000000000000000000, 1.000000000000000000, 0.000000000000000000 ) ) ;
#15931 = CARTESIAN_POINT ( 'NONE',  ( 0.2564944395515637576, -0.4441657790108029524, 1.747047244094488194 ) ) ;
#15932 = PRODUCT_CONTEXT ( 'NONE', #19177, 'mechanical' ) ;
#15933 = CARTESIAN_POINT ( 'NONE',  ( 0.4441657790107835790, 0.2564944395515610931, 1.766732283464566899 ) ) ;
#15934 = VERTEX_POINT ( 'NONE', #17829 ) ;
#15935 = DIRECTION ( 'NONE',  ( -1.000000000000000000, 0.000000000000000000, 0.000000000000000000 ) ) ;
#15936 = CONICAL_SURFACE ( 'NONE', #5095, 0.04546065111729338803, 1.047197549999998811 ) ;
#15937 = ORIENTED_EDGE ( 'NONE', *, *, #8802, .F. ) ;
#15938 = DIRECTION ( 'NONE',  ( 1.000000000000000000, 0.000000000000000000, 0.000000000000000000 ) ) ;
#15939 = ORIENTED_EDGE ( 'NONE', *, *, #24237, .F. ) ;
#15940 = EDGE_CURVE ( 'NONE', #8070, #24688, #1823, .T. ) ;
#15941 = AXIS2_PLACEMENT_3D ( 'NONE', #19947, #24733, #3113 ) ;
#15942 = CARTESIAN_POINT ( 'NONE',  ( -0.4423390553432505201, 0.2180862235769355506, -1.569881889763779625 ) ) ;
#15943 = DIRECTION ( 'NONE',  ( -1.000000000000000000, 0.000000000000000000, 0.000000000000000000 ) ) ;
#15944 = ORIENTED_EDGE ( 'NONE', *, *, #21568, .F. ) ;
#15945 = CARTESIAN_POINT ( 'NONE',  ( 0.1775991818008549328, -0.5230301363771188150, 0.9399606299212598381 ) ) ;
#15946 = ORIENTED_EDGE ( 'NONE', *, *, #21977, .F. ) ;
#15947 = ORIENTED_EDGE ( 'NONE', *, *, #6964, .T. ) ;
#15948 = ADVANCED_FACE ( 'NONE', ( #26876 ), #7451, .F. ) ;
#15949 = DIRECTION ( 'NONE',  ( -1.000000000000000000, 0.000000000000000000, 0.000000000000000000 ) ) ;
#15950 = AXIS2_PLACEMENT_3D ( 'NONE', #26377, #41, #8873 ) ;
#15951 = CARTESIAN_POINT ( 'NONE',  ( 0.1230388948667178323, -0.3365682031943129648, 0.09506557083416242171 ) ) ;
#15952 = CONTEXT_DEPENDENT_SHAPE_REPRESENTATION ( #15754, #14137 ) ;
#15953 = DIRECTION ( 'NONE',  ( 0.000000000000000000, -1.000000000000000000, 0.000000000000000000 ) ) ;
#15954 = CIRCLE ( 'NONE', #14150, 0.4247824285122252519 ) ;
#15955 = DIRECTION ( 'NONE',  ( 0.000000000000000000, 1.000000000000000000, 0.000000000000000000 ) ) ;
#15956 = DIRECTION ( 'NONE',  ( 0.000000000000000000, 0.000000000000000000, 1.000000000000000000 ) ) ;
#15957 = ORIENTED_EDGE ( 'NONE', *, *, #16581, .F. ) ;
#15958 = CARTESIAN_POINT ( 'NONE',  ( -0.4622619257814448712, 0.08092139668561793009, 0.1992125984251968684 ) ) ;
#15959 = DIRECTION ( 'NONE',  ( 1.000000000000000000, 0.000000000000000000, 0.000000000000000000 ) ) ;
#15960 = ( REPRESENTATION_RELATIONSHIP ('NONE','NONE', #12434, #6338 ) REPRESENTATION_RELATIONSHIP_WITH_TRANSFORMATION ( #20331 )SHAPE_REPRESENTATION_RELATIONSHIP( ) ) ;
#15961 = CARTESIAN_POINT ( 'NONE',  ( 0.4713455951422338974, -0.1082342125229829866, 0.2715646632666751659 ) ) ;
#15962 = CARTESIAN_POINT ( 'NONE',  ( 0.2211428102655795813, -0.2521176338356631019, 1.953740157480315043 ) ) ;
#15963 = CIRCLE ( 'NONE', #11006, 0.3584231247409862542 ) ;
#15964 = EDGE_CURVE ( 'NONE', #20796, #24033, #1158, .T. ) ;
#15965 = ORIENTED_EDGE ( 'NONE', *, *, #22642, .T. ) ;
#15966 = DIRECTION ( 'NONE',  ( 0.000000000000000000, 0.000000000000000000, 1.000000000000000000 ) ) ;
#15967 = DIRECTION ( 'NONE',  ( 0.000000000000000000, 0.000000000000000000, -1.000000000000000000 ) ) ;
#15968 = CARTESIAN_POINT ( 'NONE',  ( -0.3149606299212598381, 0.000000000000000000, -0.03543307086614173179 ) ) ;
#15969 = CARTESIAN_POINT ( 'NONE',  ( 0.1610509776512594748, -0.4407912692718567449, 0.1992125984251968684 ) ) ;
#15970 = CARTESIAN_POINT ( 'NONE',  ( 0.1136811023622047168, 0.000000000000000000, 0.09679133858267717494 ) ) ;
#15971 = DIRECTION ( 'NONE',  ( 0.000000000000000000, 0.000000000000000000, -1.000000000000000000 ) ) ;
#15972 = CARTESIAN_POINT ( 'NONE',  ( -0.1318897637674583401, 0.000000000000000000, -4.330708661396418080 ) ) ;
#15973 = CARTESIAN_POINT ( 'NONE',  ( 0.000000000000000000, 0.000000000000000000, 0.1322834645669291320 ) ) ;
#15974 = AXIS2_PLACEMENT_3D ( 'NONE', #17405, #6955, #6817 ) ;
#15975 = ( NAMED_UNIT ( * ) SI_UNIT ( $, .STERADIAN. ) SOLID_ANGLE_UNIT ( ) ) ;
#15976 = ORIENTED_EDGE ( 'NONE', *, *, #6046, .T. ) ;
#15977 = DIRECTION ( 'NONE',  ( 1.000000000000000000, 0.000000000000000000, 0.000000000000000000 ) ) ;
#15978 = CARTESIAN_POINT ( 'NONE',  ( -0.5949363243629232079, -0.1357903337134990229, 0.2362204724409449064 ) ) ;
#15979 = CARTESIAN_POINT ( 'NONE',  ( -0.3119936278838151833, -0.6460736482360152078, 0.3122824329320355030 ) ) ;
#15980 = CARTESIAN_POINT ( 'NONE',  ( -0.07874015748031511219, 0.1968503937007873850, -3.548228346456693050 ) ) ;
#15981 = VERTEX_POINT ( 'NONE', #7527 ) ;
#15982 = EDGE_CURVE ( 'NONE', #21174, #7932, #2845, .T. ) ;
#15983 = CIRCLE ( 'NONE', #19607, 0.8267716535433071723 ) ;
#15984 = ORIENTED_EDGE ( 'NONE', *, *, #1223, .T. ) ;
#15985 = EDGE_CURVE ( 'NONE', #15279, #21681, #26051, .T. ) ;
#15986 = CARTESIAN_POINT ( 'NONE',  ( 0.7873253891977465280, 0.2498443136803698561, -0.2803400842404824567 ) ) ;
#15987 = AXIS2_PLACEMENT_3D ( 'NONE', #6639, #2776, #15262 ) ;
#15988 = CARTESIAN_POINT ( 'NONE',  ( -0.09855118063547704810, 0.3667122560601320247, -3.100567304031763172 ) ) ;
#15989 = DIRECTION ( 'NONE',  ( 0.000000000000000000, 0.000000000000000000, -1.000000000000000000 ) ) ;
#15990 = CARTESIAN_POINT ( 'NONE',  ( -1.466875984251968630E-17, 0.000000000000000000, 0.000000000000000000 ) ) ;
#15991 = AXIS2_PLACEMENT_3D ( 'NONE', #10430, #19045, #27679 ) ;
#15992 = ORIENTED_EDGE ( 'NONE', *, *, #26466, .T. ) ;
#15993 = ORIENTED_EDGE ( 'NONE', *, *, #20181, .F. ) ;
#15994 = CARTESIAN_POINT ( 'NONE',  ( 0.1482986320106399469, 0.3007905576423889893, 1.973425196850393970 ) ) ;
#15995 = FACE_OUTER_BOUND ( 'NONE', #5842, .T. ) ;
#15996 = CARTESIAN_POINT ( 'NONE',  ( -0.4856708409191340392, 0.1649135259639384898, -1.550196850393700920 ) ) ;
#15997 = CARTESIAN_POINT ( 'NONE',  ( -0.5511811023622047445, 3.375010863791918375E-17, 0.9202755905511811330 ) ) ;
#15998 = FACE_BOUND ( 'NONE', #1122, .T. ) ;
#15999 = CARTESIAN_POINT ( 'NONE',  ( -0.4783323773986509764, -0.2762247810519017355, 0.9202755905511811330 ) ) ;
#16000 = CARTESIAN_POINT ( 'NONE',  ( 0.1490609433615242285, 0.000000000000000000, 0.000000000000000000 ) ) ;
#16001 = CARTESIAN_POINT ( 'NONE',  ( 0.1180276236025433051, -0.3257325899126712332, 0.1276989850574599683 ) ) ;
#16002 = CARTESIAN_POINT ( 'NONE',  ( -0.06420467502049352626, 0.05385271582827238362, -0.4702630791244896691 ) ) ;
#16003 = VECTOR ( 'NONE', #21433, 39.37007874015748143 ) ;
#16004 = EDGE_CURVE ( 'NONE', #9013, #27602, #7188, .T. ) ;
#16005 = ( NAMED_UNIT ( * ) PLANE_ANGLE_UNIT ( ) SI_UNIT ( $, .RADIAN. ) ) ;
#16006 = CARTESIAN_POINT ( 'NONE',  ( -0.4333973147258542991, -0.2509079296564011852, 0.09685039370078740717 ) ) ;
#16007 = DIRECTION ( 'NONE',  ( 0.000000000000000000, -1.000000000000000000, 0.000000000000000000 ) ) ;
#16008 = DIRECTION ( 'NONE',  ( 0.000000000000000000, 0.000000000000000000, 1.000000000000000000 ) ) ;
#16009 = ORIENTED_EDGE ( 'NONE', *, *, #676, .F. ) ;
#16010 = EDGE_LOOP ( 'NONE', ( #24861, #20462, #1138, #330 ) ) ;
#16011 = VECTOR ( 'NONE', #22821, 39.37007874015748854 ) ;
#16012 = CIRCLE ( 'NONE', #26838, 0.09143349766193348271 ) ;
#16013 = SPHERICAL_SURFACE ( 'NONE', #13818, 0.1003956692913385851 ) ;
#16014 = DIRECTION ( 'NONE',  ( -1.000000000000000000, 0.000000000000000000, 0.000000000000000000 ) ) ;
#16015 = ORIENTED_EDGE ( 'NONE', *, *, #14275, .F. ) ;
#16016 = CARTESIAN_POINT ( 'NONE',  ( 0.2669917830071264486, 0.2341095169845867630, 1.953740157480315487 ) ) ;
#16017 = ORIENTED_EDGE ( 'NONE', *, *, #20971, .F. ) ;
#16018 = CARTESIAN_POINT ( 'NONE',  ( 0.3929158813954875540, -0.2268989272875726881, -1.934055118110236338 ) ) ;
#16019 = CARTESIAN_POINT ( 'NONE',  ( -0.4149306118461465465, -0.2388850582578584125, 0.08349695147705923914 ) ) ;
#16020 = CARTESIAN_POINT ( 'NONE',  ( -0.4932821129636645874, 0.08637579872942342807, 0.09685039370078740717 ) ) ;
#16021 = CARTESIAN_POINT ( 'NONE',  ( 0.02573923578592207315, 0.3139710921709522595, -3.177418918035737949 ) ) ;
#16022 = DIRECTION ( 'NONE',  ( 0.000000000000000000, 0.000000000000000000, -1.000000000000000000 ) ) ;
#16023 = VERTEX_POINT ( 'NONE', #12187 ) ;
#16024 = AXIS2_PLACEMENT_3D ( 'NONE', #13180, #9077, #19697 ) ;
#16025 = DIRECTION ( 'NONE',  ( -1.000000000000000000, -1.224646799147356165E-16, 0.000000000000000000 ) ) ;
#16026 = CARTESIAN_POINT ( 'NONE',  ( -0.4219262446670208888, -0.1431849087164892009, -1.934055118110236116 ) ) ;
#16027 = CARTESIAN_POINT ( 'NONE',  ( 0.3384212623783066642, -0.1668516812751465739, -3.100567304031770277 ) ) ;
#16028 = DIRECTION ( 'NONE',  ( -1.000000000000000000, 0.000000000000000000, 0.000000000000000000 ) ) ;
#16029 = B_SPLINE_CURVE_WITH_KNOTS ( 'NONE', 3,
 ( #1240, #1369, #13950, #7875, #7737, #20303 ),
 .UNSPECIFIED., .F., .F.,
 ( 4, 2, 4 ),
 ( 0.5000000000000000000, 0.7500000000000000000, 1.000000000000000000 ),
 .UNSPECIFIED. ) ;
#16030 = DIRECTION ( 'NONE',  ( 0.000000000000000000, 0.000000000000000000, 1.000000000000000000 ) ) ;
#16031 = ORIENTED_EDGE ( 'NONE', *, *, #24591, .F. ) ;
#16032 = CARTESIAN_POINT ( 'NONE',  ( -0.4446020952038907681, 0.000000000000000000, -1.934055118110236338 ) ) ;
#16033 = AXIS2_PLACEMENT_3D ( 'NONE', #17551, #19251, #15449 ) ;
#16034 = CIRCLE ( 'NONE', #15153, 0.1673228346456692994 ) ;
#16035 = CARTESIAN_POINT ( 'NONE',  ( -0.3454440660767502114, -0.3030032861725112103, -1.928289503579147635 ) ) ;
#16036 = PRODUCT_CONTEXT ( 'NONE', #3483, 'mechanical' ) ;
#16037 = EDGE_CURVE ( 'NONE', #15630, #5827, #11980, .T. ) ;
#16038 = DIRECTION ( 'NONE',  ( 1.000000000000000000, 0.000000000000000000, 0.000000000000000000 ) ) ;
#16039 = VERTEX_POINT ( 'NONE', #23513 ) ;
#16040 = CARTESIAN_POINT ( 'NONE',  ( -0.3861436020174326966, -1.005626036844328830, -0.2420500664475239982 ) ) ;
#16041 = LINE ( 'NONE', #648, #12221 ) ;
#16042 = CARTESIAN_POINT ( 'NONE',  ( -0.5085118447801415531, -0.06699507805368200286, 1.747047244094488194 ) ) ;
#16043 = EDGE_CURVE ( 'NONE', #26494, #25584, #10485, .T. ) ;
#16044 = DIRECTION ( 'NONE',  ( 0.000000000000000000, 1.000000000000000000, 0.000000000000000000 ) ) ;
#16045 = EDGE_LOOP ( 'NONE', ( #5451, #7646, #5727, #7686, #22033, #4647, #7315, #12016, #16470, #7920, #13466 ) ) ;
#16046 = ORIENTED_EDGE ( 'NONE', *, *, #15791, .T. ) ;
#16047 = CARTESIAN_POINT ( 'NONE',  ( 0.1668516812751446310, 0.3384212623783090512, -3.100567304031764948 ) ) ;
#16048 = EDGE_CURVE ( 'NONE', #13016, #9428, #9638, .T. ) ;
#16049 = CARTESIAN_POINT ( 'NONE',  ( 0.7874015748031496509, 0.2607538277840750762, -0.2385700914728043909 ) ) ;
#16050 = CARTESIAN_POINT ( 'NONE',  ( -0.2602238532265429005, 0.000000000000000000, 0.2362204724409449064 ) ) ;
#16051 = EDGE_LOOP ( 'NONE', ( #8905, #22924 ) ) ;
#16052 = ORIENTED_EDGE ( 'NONE', *, *, #12492, .T. ) ;
#16053 = CARTESIAN_POINT ( 'NONE',  ( -0.3611053385039311725, -0.7050837974523566087, -0.6410818428499839294 ) ) ;
#16054 = ORIENTED_EDGE ( 'NONE', *, *, #21603, .F. ) ;
#16055 = LINE ( 'NONE', #18135, #23947 ) ;
#16056 = AXIS2_PLACEMENT_3D ( 'NONE', #26421, #20356, #20208 ) ;
#16057 = ORIENTED_EDGE ( 'NONE', *, *, #16884, .F. ) ;
#16058 = CARTESIAN_POINT ( 'NONE',  ( 0.05819755867304853003, -0.4417361510194242613, -1.934055118110236338 ) ) ;
#16059 = EDGE_LOOP ( 'NONE', ( #8202, #17312 ) ) ;
#16060 = CARTESIAN_POINT ( 'NONE',  ( -0.6633461167951516524, 0.02596910924942653909, 0.2360419752028775631 ) ) ;
#16061 = LINE ( 'NONE', #24655, #25286 ) ;
#16062 = CIRCLE ( 'NONE', #15607, 0.8267716535433071723 ) ;
#16063 = CARTESIAN_POINT ( 'NONE',  ( 0.2083728861314909642, 0.4507717232072007696, -0.1539094607187527497 ) ) ;
#16064 = CARTESIAN_POINT ( 'NONE',  ( 0.02063524494269815615, 0.1968503937007874127, -3.195960501083794814 ) ) ;
#16065 = DIRECTION ( 'NONE',  ( -1.000000000000000000, 0.000000000000000000, 0.000000000000000000 ) ) ;
#16066 = CARTESIAN_POINT ( 'NONE',  ( -0.1685339107540412551, 0.2924088307484719595, 1.973425196850393970 ) ) ;
#16067 = DIRECTION ( 'NONE',  ( 0.000000000000000000, 0.000000000000000000, 1.000000000000000000 ) ) ;
#16068 = FACE_OUTER_BOUND ( 'NONE', #6606, .T. ) ;
#16069 = CARTESIAN_POINT ( 'NONE',  ( -1.197070535079588716, 0.07874015748031495954, 1.315180771300060503 ) ) ;
#16070 = SURFACE_STYLE_USAGE ( .BOTH. , #3045 ) ;
#16071 = CARTESIAN_POINT ( 'NONE',  ( -0.2817310484609168997, -0.2161381151963037983, 1.953740157480315043 ) ) ;
#16072 = ORIENTED_EDGE ( 'NONE', *, *, #5952, .F. ) ;
#16073 = CARTESIAN_POINT ( 'NONE',  ( -0.5376957092749378164, -0.3112026930392873814, 0.2574803149606298969 ) ) ;
#16074 = EDGE_CURVE ( 'NONE', #14684, #21440, #7023, .T. ) ;
#16075 = DIRECTION ( 'NONE',  ( 1.000000000000000000, 0.000000000000000000, 0.000000000000000000 ) ) ;
#16076 = CARTESIAN_POINT ( 'NONE',  ( 0.000000000000000000, 0.000000000000000000, -0.006889763779527558960 ) ) ;
#16077 = CYLINDRICAL_SURFACE ( 'NONE', #14222, 0.6299212598425196763 ) ;
#16078 = CARTESIAN_POINT ( 'NONE',  ( 0.1649135259617203753, -0.4856708409200670151, 1.747047244094488194 ) ) ;
#16079 = ADVANCED_BREP_SHAPE_REPRESENTATION ( 'Deep Groove Ball Bearing 20x42x12', ( #12108, #11588 ), #1261 ) ;
#16080 = EDGE_CURVE ( 'NONE', #5524, #4811, #24587, .T. ) ;
#16081 = AXIS2_PLACEMENT_3D ( 'NONE', #905, #20387, #24339 ) ;
#16082 = VERTEX_POINT ( 'NONE', #14770 ) ;
#16083 = CARTESIAN_POINT ( 'NONE',  ( -0.3223547283257516272, 0.3832433309296771617, 0.09685039370078740717 ) ) ;
#16084 = VERTEX_POINT ( 'NONE', #3859 ) ;
#16085 = EDGE_CURVE ( 'NONE', #3868, #7482, #18724, .T. ) ;
#16086 = CARTESIAN_POINT ( 'NONE',  ( 8.353478384051541640E-17, -4.420672499999999463E-18, -0.1023622047244094474 ) ) ;
#16087 = B_SPLINE_CURVE_WITH_KNOTS ( 'NONE', 3,
 ( #21867, #6213, #1954, #19465, #25693, #4358, #13105, #10564, #21730, #14841 ),
 .UNSPECIFIED., .F., .F.,
 ( 4, 2, 2, 2, 4 ),
 ( 0.000000000000000000, 0.2499999999999998335, 0.4999999999999996669, 0.7499999999999997780, 1.000000000000000000 ),
 .UNSPECIFIED. ) ;
#16088 = CARTESIAN_POINT ( 'NONE',  ( -0.2816963220976719806, -0.2161875334156889150, 1.953740157480315043 ) ) ;
#16089 = CARTESIAN_POINT ( 'NONE',  ( -0.2362204724409449064, 0.8809055118110236116, 0.000000000000000000 ) ) ;
#16090 = VERTEX_POINT ( 'NONE', #27314 ) ;
#16091 = EDGE_LOOP ( 'NONE', ( #5347, #20962, #25119, #17034, #26054 ) ) ;
#16092 = CARTESIAN_POINT ( 'NONE',  ( -0.4669911931914806358, 0.1585706980422473544, -1.569881889763779625 ) ) ;
#16093 = ORIENTED_EDGE ( 'NONE', *, *, #17507, .F. ) ;
#16094 = CARTESIAN_POINT ( 'NONE',  ( -0.2529800193559212929, 0.5131133041954029084, 0.9399606299212598381 ) ) ;
#16095 = VERTEX_POINT ( 'NONE', #5992 ) ;
#16096 = CARTESIAN_POINT ( 'NONE',  ( -0.3346456692913385988, 2.134256245050205639E-17, 1.973425196850393970 ) ) ;
#16097 = CARTESIAN_POINT ( 'NONE',  ( -0.09842519685039370636, 0.2991866959364303802, -3.548228346456693050 ) ) ;
#16098 = AXIS2_PLACEMENT_3D ( 'NONE', #25137, #25422, #21039 ) ;
#16099 = ITEM_DEFINED_TRANSFORMATION ( 'NONE', 'NONE', #16524,  #11588 ) ;
#16100 = AXIS2_PLACEMENT_3D ( 'NONE', #12368, #27637, #23682 ) ;
#16101 = DIRECTION ( 'NONE',  ( -1.000000000000000000, 0.000000000000000000, 0.000000000000000000 ) ) ;
#16102 = DIRECTION ( 'NONE',  ( 0.000000000000000000, -1.000000000000000000, 0.000000000000000000 ) ) ;
#16103 = DIRECTION ( 'NONE',  ( 8.659560570126445370E-17, 0.7071067805519554161, -0.7071067818211396183 ) ) ;
#16104 = CARTESIAN_POINT ( 'NONE',  ( -0.5677441908128971759, 0.6261827486008704202, 0.07772707057083097504 ) ) ;
#16105 = LINE ( 'NONE', #13988, #6587 ) ;
#16106 = CIRCLE ( 'NONE', #20619, 0.01181102362204724046 ) ;
#16107 = FACE_OUTER_BOUND ( 'NONE', #7719, .T. ) ;
#16108 = ORIENTED_EDGE ( 'NONE', *, *, #4192, .T. ) ;
#16109 = FACE_OUTER_BOUND ( 'NONE', #18924, .T. ) ;
#16110 = CARTESIAN_POINT ( 'NONE',  ( -0.3191377210039603174, 0.3812612458993721587, 0.1615162260891281343 ) ) ;
#16111 = EDGE_CURVE ( 'NONE', #5538, #16472, #14978, .T. ) ;
#16112 = FACE_OUTER_BOUND ( 'NONE', #23545, .T. ) ;
#16113 = CARTESIAN_POINT ( 'NONE',  ( 0.2078289949484098675, -0.4330237525398077381, 0.2529987172081292757 ) ) ;
#16114 = CARTESIAN_POINT ( 'NONE',  ( 2.186367668367731174E-17, 0.3771653543307086909, 0.1992150590373740204 ) ) ;
#16115 = CARTESIAN_POINT ( 'NONE',  ( 0.1490609433615240342, -0.2393035190771456711, 0.4144858534716441278 ) ) ;
#16116 = EDGE_CURVE ( 'NONE', #7932, #8713, #27601, .T. ) ;
#16117 = CARTESIAN_POINT ( 'NONE',  ( -0.2208527687073504053, -0.6048181665964218467, 0.2359405056213304541 ) ) ;
#16118 = ORIENTED_EDGE ( 'NONE', *, *, #5679, .T. ) ;
#16119 = AXIS2_PLACEMENT_3D ( 'NONE', #10596, #19219, #10745 ) ;
#16120 = ORIENTED_EDGE ( 'NONE', *, *, #23921, .T. ) ;
#16121 = ( LENGTH_UNIT ( ) NAMED_UNIT ( * ) SI_UNIT ( $, .METRE. ) ) ;
#16122 = EDGE_CURVE ( 'NONE', #18410, #10904, #4748, .T. ) ;
#16123 = ORIENTED_EDGE ( 'NONE', *, *, #17628, .F. ) ;
#16124 = DIRECTION ( 'NONE',  ( -1.000000000000000000, 0.000000000000000000, 0.000000000000000000 ) ) ;
#16125 = CARTESIAN_POINT ( 'NONE',  ( -0.1870078740157480324, 0.000000000000000000, 0.000000000000000000 ) ) ;
#16126 = CARTESIAN_POINT ( 'NONE',  ( -0.09842519684999369300, 0.1968503937007873850, -3.561114497143084368 ) ) ;
#16127 = ORIENTED_EDGE ( 'NONE', *, *, #23073, .F. ) ;
#16128 = CARTESIAN_POINT ( 'NONE',  ( -0.3411065095061437957, 0.06065137456822555090, 0.1377952755905512139 ) ) ;
#16129 = DIRECTION ( 'NONE',  ( 1.000000000000000000, 0.000000000000000000, 0.000000000000000000 ) ) ;
#16130 = ORIENTED_EDGE ( 'NONE', *, *, #6942, .T. ) ;
#16131 = CARTESIAN_POINT ( 'NONE',  ( 0.4337933494688747671, -0.2502226818840338485, 0.2574827755769819038 ) ) ;
#16132 = DIRECTION ( 'NONE',  ( 0.000000000000000000, 0.000000000000000000, 1.000000000000000000 ) ) ;
#16133 = CARTESIAN_POINT ( 'NONE',  ( 0.5309636003393858328, 0.6324615022621647986, -0.5368779841232129701 ) ) ;
#16134 = AXIS2_PLACEMENT_3D ( 'NONE', #3677, #14448, #14595 ) ;
#16135 = CARTESIAN_POINT ( 'NONE',  ( -0.1896185148830509259, 0.3289909311256231650, -3.100567304031763172 ) ) ;
#16136 = FACE_OUTER_BOUND ( 'NONE', #7059, .T. ) ;
#16137 = LINE ( 'NONE', #7510, #5639 ) ;
#16138 = AXIS2_PLACEMENT_3D ( 'NONE', #25176, #7680, #12324 ) ;
#16139 = EDGE_LOOP ( 'NONE', ( #9181, #14269 ) ) ;
#16140 = AXIS2_PLACEMENT_3D ( 'NONE', #20683, #22952, #18686 ) ;
#16141 = CARTESIAN_POINT ( 'NONE',  ( 0.3346456692913385988, 0.000000000000000000, 1.973425196850393970 ) ) ;
#16142 = CARTESIAN_POINT ( 'NONE',  ( -0.3855916753034290823, 0.3382184156749268311, -1.550196850393700920 ) ) ;
#16143 = CARTESIAN_POINT ( 'NONE',  ( -0.3713752547280854133, 0.06583429795695157349, 0.07637630750536809898 ) ) ;
#16144 = ADVANCED_FACE ( 'NONE', ( #4681 ), #6406, .F. ) ;
#16145 = DIRECTION ( 'NONE',  ( -0.000000000000000000, 1.000000000000000000, -0.000000000000000000 ) ) ;
#16146 = VERTEX_POINT ( 'NONE', #2286 ) ;
#16147 = CARTESIAN_POINT ( 'NONE',  ( -0.04448665381632212201, 0.06523692067838750275, -0.4653551329966305605 ) ) ;
#16148 = EDGE_CURVE ( 'NONE', #2247, #5635, #26030, .T. ) ;
#16149 = CARTESIAN_POINT ( 'NONE',  ( -0.1585706980422471879, 0.4669911931914806913, -1.569881889763779625 ) ) ;
#16150 = EDGE_CURVE ( 'NONE', #339, #18410, #3116, .T. ) ;
#16151 = FACE_OUTER_BOUND ( 'NONE', #21824, .T. ) ;
#16152 = CARTESIAN_POINT ( 'NONE',  ( 0.000000000000000000, 0.000000000000000000, 0.2362204724409449064 ) ) ;
#16153 = DIRECTION ( 'NONE',  ( 0.000000000000000000, 1.000000000000000000, 0.000000000000000000 ) ) ;
#16154 = AXIS2_PLACEMENT_3D ( 'NONE', #5358, #26402, #9295 ) ;
#16155 = ORIENTED_EDGE ( 'NONE', *, *, #17686, .T. ) ;
#16156 = AXIS2_PLACEMENT_3D ( 'NONE', #10696, #17197, #25816 ) ;
#16157 = LENGTH_MEASURE_WITH_UNIT ( LENGTH_MEASURE( 0.02539999999999999897 ), #19032 ) ;
#16158 = DIRECTION ( 'NONE',  ( 1.000000000000000000, 0.000000000000000000, 0.000000000000000000 ) ) ;
#16159 = AXIS2_PLACEMENT_3D ( 'NONE', #15879, #3286, #24484 ) ;
#16160 = PRODUCT_DEFINITION_SHAPE ( 'NONE', 'NONE',  #27892 ) ;
#16161 = FACE_OUTER_BOUND ( 'NONE', #26776, .T. ) ;
#16162 = ORIENTED_EDGE ( 'NONE', *, *, #23187, .T. ) ;
#16163 = CARTESIAN_POINT ( 'NONE',  ( -0.2341095169845849588, 0.2669917830071098508, 1.953740157480314821 ) ) ;
#16164 = ORIENTED_EDGE ( 'NONE', *, *, #21663, .T. ) ;
#16165 = DIRECTION ( 'NONE',  ( 0.000000000000000000, -1.000000000000000000, 0.000000000000000000 ) ) ;
#16166 = CYLINDRICAL_SURFACE ( 'NONE', #12487, 0.6299212598425196763 ) ;
#16167 = CARTESIAN_POINT ( 'NONE',  ( 0.1522836969735573143, -0.2938892803217901806, -0.3971963147566889840 ) ) ;
#16168 = CIRCLE ( 'NONE', #16624, 0.5007874015748031704 ) ;
#16169 = CARTESIAN_POINT ( 'NONE',  ( 0.3986320731132086959, -0.2308081338369904478, 0.1771653543307089018 ) ) ;
#16170 = PLANE ( 'NONE',  #15839 ) ;
#16171 = CARTESIAN_POINT ( 'NONE',  ( 0.4898768902087983768, -1.617596456692913393E-16, -0.07874015748031495954 ) ) ;
#16172 = VERTEX_POINT ( 'NONE', #21934 ) ;
#16173 = DIRECTION ( 'NONE',  ( 0.000000000000000000, 0.000000000000000000, 1.000000000000000000 ) ) ;
#16174 = DIRECTION ( 'NONE',  ( 0.000000000000000000, -1.000000000000000000, 0.000000000000000000 ) ) ;
#16175 = CARTESIAN_POINT ( 'NONE',  ( -5.747161356628524594E-17, -0.4692913385826771866, 0.2374015748031496065 ) ) ;
#16176 = CARTESIAN_POINT ( 'NONE',  ( -0.2488091035917020799, -0.2836590635674518524, -3.100567304031764948 ) ) ;
#16177 = TOROIDAL_SURFACE ( 'NONE', #6698, 0.4980314960629921295, 0.01377952755905511792 ) ;
#16178 = ORIENTED_EDGE ( 'NONE', *, *, #19204, .F. ) ;
#16179 = CARTESIAN_POINT ( 'NONE',  ( -0.4382752542996525835, 0.1173917140416343985, -1.934055118110236338 ) ) ;
#16180 = CIRCLE ( 'NONE', #19321, 0.4786070381542913421 ) ;
#16181 = AXIS2_PLACEMENT_3D ( 'NONE', #4821, #13437, #23657 ) ;
#16182 = ADVANCED_FACE ( 'NONE', ( #6959, #87 ), #2556, .T. ) ;
#16183 = CIRCLE ( 'NONE', #26545, 0.02362204724409448092 ) ;
#16184 = CARTESIAN_POINT ( 'NONE',  ( -0.4280150452258433269, -0.6326300546481929965, -0.3109213582405842557 ) ) ;
#16185 = DIRECTION ( 'NONE',  ( 0.000000000000000000, 0.000000000000000000, -1.000000000000000000 ) ) ;
#16186 = CARTESIAN_POINT ( 'NONE',  ( 0.2268096725222282783, -0.4600326175560538466, 1.747047244094488194 ) ) ;
#16187 = B_SPLINE_CURVE_WITH_KNOTS ( 'NONE', 3,
 ( #8297, #25525, #25663, #6317 ),
 .UNSPECIFIED., .F., .F.,
 ( 4, 4 ),
 ( 0.9101643785100869133, 1.000000000000000000 ),
 .UNSPECIFIED. ) ;
#16188 = VERTEX_POINT ( 'NONE', #19535 ) ;
#16189 = ORIENTED_EDGE ( 'NONE', *, *, #23474, .F. ) ;
#16190 = CARTESIAN_POINT ( 'NONE',  ( 0.3572819248074444731, 0.1213180142433879782, -3.100567304031760951 ) ) ;
#16191 = ORIENTED_EDGE ( 'NONE', *, *, #5518, .T. ) ;
#16192 = CARTESIAN_POINT ( 'NONE',  ( -0.6003937007829848183, 1.122047244090071727, 1.315345636034250449E-15 ) ) ;
#16193 = CYLINDRICAL_SURFACE ( 'NONE', #8685, 0.5322834645669292097 ) ;
#16194 = VERTEX_POINT ( 'NONE', #346 ) ;
#16195 = CARTESIAN_POINT ( 'NONE',  ( -0.1648264847745520012, 0.4857053587578358256, -1.550196850393700920 ) ) ;
#16196 = CARTESIAN_POINT ( 'NONE',  ( -0.4223526811679828574, -0.5446405551315159910, -0.4444161484266240802 ) ) ;
#16197 = VECTOR ( 'NONE', #3480, 39.37007874015748143 ) ;
#16198 = DIRECTION ( 'NONE',  ( 0.000000000000000000, 0.000000000000000000, 1.000000000000000000 ) ) ;
#16199 = CIRCLE ( 'NONE', #27027, 0.4692913385826771866 ) ;
#16200 = ORIENTED_EDGE ( 'NONE', *, *, #13134, .T. ) ;
#16201 = ORIENTED_EDGE ( 'NONE', *, *, #11636, .F. ) ;
#16202 = ADVANCED_FACE ( 'NONE', ( #10915 ), #13767, .F. ) ;
#16203 = CARTESIAN_POINT ( 'NONE',  ( -0.7432982829791772161, 0.3208553412839740826, 0.1963361843227200976 ) ) ;
#16204 = DIRECTION ( 'NONE',  ( -0.000000000000000000, -0.000000000000000000, 1.000000000000000000 ) ) ;
#16205 = EDGE_CURVE ( 'NONE', #22689, #14042, #22813, .T. ) ;
#16206 = CARTESIAN_POINT ( 'NONE',  ( -0.2490711204941342405, 1.208528701367826752, -0.6047752023237676910 ) ) ;
#16207 = VECTOR ( 'NONE', #17278, 39.37007874015748143 ) ;
#16208 = CARTESIAN_POINT ( 'NONE',  ( 0.5075887755601056206, 1.024205082384598509, -0.2696197026301838107 ) ) ;
#16209 = CARTESIAN_POINT ( 'NONE',  ( 0.03532354024591712049, -0.8267716535433071723, -0.8267716535433071723 ) ) ;
#16210 = ADVANCED_FACE ( 'NONE', ( #13029 ), #17387, .F. ) ;
#16211 = CARTESIAN_POINT ( 'NONE',  ( -0.3184841198566448206, 0.1570220809524502381, 1.953740157480315043 ) ) ;
#16212 = EDGE_LOOP ( 'NONE', ( #18481, #15807, #428, #9788, #16754 ) ) ;
#16213 = CARTESIAN_POINT ( 'NONE',  ( 0.000000000000000000, 0.000000000000000000, 0.1771653543307086520 ) ) ;
#16214 = CARTESIAN_POINT ( 'NONE',  ( -0.4930758245789425009, 0.08754571829529331217, 0.09685039370078740717 ) ) ;
#16215 = CARTESIAN_POINT ( 'NONE',  ( 0.1447526197146039584, -0.3977045540727763839, 0.1377952755905511861 ) ) ;
#16216 = CARTESIAN_POINT ( 'NONE',  ( 0.3220512119205940493, 0.3834984712787528061, 0.09684793308443542803 ) ) ;
#16217 = VECTOR ( 'NONE', #8017, 39.37007874015748143 ) ;
#16218 = CARTESIAN_POINT ( 'NONE',  ( -0.4858607088160732390, -0.2805118110236220486, 0.1771653543307086520 ) ) ;
#16219 = VERTEX_POINT ( 'NONE', #24184 ) ;
#16220 = AXIS2_PLACEMENT_3D ( 'NONE', #12106, #3912, #10404 ) ;
#16221 = CARTESIAN_POINT ( 'NONE',  ( 3.606039370078740678E-16, -0.6299212598425196763, 0.000000000000000000 ) ) ;
#16222 = CARTESIAN_POINT ( 'NONE',  ( -0.1712563538833084820, -0.5043504886477717664, 1.747047244094488194 ) ) ;
#16223 = CARTESIAN_POINT ( 'NONE',  ( 0.2268096725222696064, 0.4600326175561003650, 1.747047244094488194 ) ) ;
#16224 = ORIENTED_EDGE ( 'NONE', *, *, #17233, .T. ) ;
#16225 = DIRECTION ( 'NONE',  ( 0.000000000000000000, 1.000000000000000000, 0.000000000000000000 ) ) ;
#16226 = EDGE_LOOP ( 'NONE', ( #24644, #3517, #7694, #23020, #11131, #2557 ) ) ;
#16227 = CARTESIAN_POINT ( 'NONE',  ( -0.1771653543307086520, -5.663984251968503442E-18, 0.000000000000000000 ) ) ;
#16228 = ( NAMED_UNIT ( * ) PLANE_ANGLE_UNIT ( ) SI_UNIT ( $, .RADIAN. ) ) ;
#16229 = FACE_OUTER_BOUND ( 'NONE', #17870, .T. ) ;
#16230 = DIRECTION ( 'NONE',  ( 1.000000000000000000, 0.000000000000000000, 0.000000000000000000 ) ) ;
#16231 = ORIENTED_EDGE ( 'NONE', *, *, #4506, .T. ) ;
#16232 = SHAPE_REPRESENTATION ( 'M6 Thin Hex Nut', ( #11588 ), #15695 ) ;
#16233 = VERTEX_POINT ( 'NONE', #15580 ) ;
#16234 = EDGE_CURVE ( 'NONE', #26492, #2487, #4283, .T. ) ;
#16235 = CARTESIAN_POINT ( 'NONE',  ( -0.4763861460130343062, -0.1275996891957688339, -1.569881889763779625 ) ) ;
#16236 = CARTESIAN_POINT ( 'NONE',  ( 0.4333973147258542991, -0.2509079296564015737, 0.09685039370078740717 ) ) ;
#16237 = VERTEX_POINT ( 'NONE', #2015 ) ;
#16238 = ORIENTED_EDGE ( 'NONE', *, *, #10013, .F. ) ;
#16239 = TOROIDAL_SURFACE ( 'NONE', #12165, 0.1023622047244094474, 0.003937007874015747977 ) ;
#16240 = VECTOR ( 'NONE', #4054, 39.37007874015748143 ) ;
#16241 = DIRECTION ( 'NONE',  ( -1.000000000000000000, 0.000000000000000000, 0.000000000000000000 ) ) ;
#16242 = ADVANCED_FACE ( 'NONE', ( #13429 ), #11072, .T. ) ;
#16243 = CARTESIAN_POINT ( 'NONE',  ( 0.000000000000000000, 0.03937007874015747977, -0.3937007874015748254 ) ) ;
#16244 = DIRECTION ( 'NONE',  ( 0.000000000000000000, 0.000000000000000000, -1.000000000000000000 ) ) ;
#16245 = DIRECTION ( 'NONE',  ( 0.000000000000000000, 0.000000000000000000, 1.000000000000000000 ) ) ;
#16246 = EDGE_CURVE ( 'NONE', #26179, #20180, #4826, .T. ) ;
#16247 = ORIENTED_EDGE ( 'NONE', *, *, #17918, .F. ) ;
#16248 = DIRECTION ( 'NONE',  ( 0.7660444431189775694, -0.6427876096865398070, 0.000000000000000000 ) ) ;
#16249 = ADVANCED_FACE ( 'NONE', ( #21656 ), #9460, .T. ) ;
#16250 = CARTESIAN_POINT ( 'NONE',  ( 0.3346456692913385988, -0.02190250779246876237, 1.953740157480315043 ) ) ;
#16251 = ORIENTED_EDGE ( 'NONE', *, *, #6742, .F. ) ;
#16252 = CARTESIAN_POINT ( 'NONE',  ( -0.4620608682196457040, 0.08206165078054665496, 0.07637795275590551769 ) ) ;
#16253 = CARTESIAN_POINT ( 'NONE',  ( 2.664928230027803213, -0.4724409448818898127, 0.8182917201112815953 ) ) ;
#16254 = DIRECTION ( 'NONE',  ( -1.000000000000000000, 0.000000000000000000, 0.000000000000000000 ) ) ;
#16255 = CARTESIAN_POINT ( 'NONE',  ( -0.4021324607151492980, 0.3215300179757064614, 0.1473214333199995008 ) ) ;
#16256 = TOROIDAL_SURFACE ( 'NONE', #15689, 0.4232283464566928832, 0.07677165354330708902 ) ;
#16257 = TOROIDAL_SURFACE ( 'NONE', #25268, 0.4232283464566928832, 0.07677165354330708902 ) ;
#16258 = ORIENTED_EDGE ( 'NONE', *, *, #25744, .F. ) ;
#16259 = ORIENTED_EDGE ( 'NONE', *, *, #14708, .F. ) ;
#16260 = EDGE_LOOP ( 'NONE', ( #20414, #19061, #24901, #1662 ) ) ;
#16261 = CIRCLE ( 'NONE', #9477, 0.07677362204724409722 ) ;
#16262 = CARTESIAN_POINT ( 'NONE',  ( 0.3976891862754212137, 1.133679329692560245, -0.4395307839725697274 ) ) ;
#16263 = DIRECTION ( 'NONE',  ( 1.000000000000000000, 0.000000000000000000, 0.000000000000000000 ) ) ;
#16264 = DIMENSIONAL_EXPONENTS ( 1.000000000000000000, 0.000000000000000000, 0.000000000000000000, 0.000000000000000000, 0.000000000000000000, 0.000000000000000000, 0.000000000000000000 ) ;
#16265 = VERTEX_POINT ( 'NONE', #2426 ) ;
#16266 = CARTESIAN_POINT ( 'NONE',  ( 0.000000000000000000, 0.07874015748031495954, 1.988188976307287970 ) ) ;
#16267 = DIRECTION ( 'NONE',  ( 1.000000000000000000, 0.000000000000000000, 0.000000000000000000 ) ) ;
#16268 = ORIENTED_EDGE ( 'NONE', *, *, #13152, .F. ) ;
#16269 = EDGE_CURVE ( 'NONE', #15613, #9254, #24354, .T. ) ;
#16270 = B_SPLINE_CURVE_WITH_KNOTS ( 'NONE', 3,
 ( #3514, #24996, #16255, #3226, #24574, #11865, #18486, #20486 ),
 .UNSPECIFIED., .F., .F.,
 ( 4, 2, 2, 4 ),
 ( 0.000000000000000000, 0.1250000000000000000, 0.2499999999999998335, 0.5000000000000000000 ),
 .UNSPECIFIED. ) ;
#16271 = CARTESIAN_POINT ( 'NONE',  ( 0.000000000000000000, 0.000000000000000000, -0.3779527559055118058 ) ) ;
#16272 = EDGE_CURVE ( 'NONE', #6594, #9793, #12174, .T. ) ;
#16273 = FACE_OUTER_BOUND ( 'NONE', #24510, .T. ) ;
#16274 = DIRECTION ( 'NONE',  ( 0.000000000000000000, 0.000000000000000000, -1.000000000000000000 ) ) ;
#16275 = ORIENTED_EDGE ( 'NONE', *, *, #21382, .T. ) ;
#16276 = ORIENTED_EDGE ( 'NONE', *, *, #5317, .T. ) ;
#16277 = CARTESIAN_POINT ( 'NONE',  ( 0.3239425792934412240, 0.08676778863010829734, 1.973425196850393970 ) ) ;
#16278 = DIRECTION ( 'NONE',  ( 0.000000000000000000, 0.000000000000000000, 1.000000000000000000 ) ) ;
#16279 = ADVANCED_FACE ( 'NONE', ( #20498 ), #14464, .F. ) ;
#16280 = CARTESIAN_POINT ( 'NONE',  ( -1.197070535079588716, 0.4724409448818898127, 1.197070535079588716 ) ) ;
#16281 = VECTOR ( 'NONE', #137, 39.37007874015748143 ) ;
#16282 = CARTESIAN_POINT ( 'NONE',  ( 0.5476281405333177643, 0.07214854559198216610, 0.9202755905511811330 ) ) ;
#16283 = DIRECTION ( 'NONE',  ( 0.000000000000000000, -0.8660254037844388186, 0.4999999999999998890 ) ) ;
#16284 = CARTESIAN_POINT ( 'NONE',  ( 0.000000000000000000, 0.000000000000000000, 0.3425196850393700809 ) ) ;
#16285 = EDGE_LOOP ( 'NONE', ( #12936, #27116, #16057, #3597, #16806, #9218, #5083 ) ) ;
#16286 = CARTESIAN_POINT ( 'NONE',  ( -0.4158785340170984557, 0.3322209827720822850, 0.3401591244667909186 ) ) ;
#16287 = CARTESIAN_POINT ( 'NONE',  ( 0.4669911931914765835, 0.1585706980422571244, -1.569881889763779625 ) ) ;
#16288 = CARTESIAN_POINT ( 'NONE',  ( 0.1516263115863346334, -0.4909405214979283838, 0.05579628926458630317 ) ) ;
#16289 = FACE_OUTER_BOUND ( 'NONE', #12179, .T. ) ;
#16290 = CARTESIAN_POINT ( 'NONE',  ( 0.5043892184459985994, 0.1711665596932881450, 1.747047244094488194 ) ) ;
#16291 = FACE_OUTER_BOUND ( 'NONE', #9157, .T. ) ;
#16292 = CARTESIAN_POINT ( 'NONE',  ( 0.3218523081053298873, -0.6665164569875627887, 0.2562996995945706069 ) ) ;
#16293 = ORIENTED_EDGE ( 'NONE', *, *, #16737, .T. ) ;
#16294 = CIRCLE ( 'NONE', #7729, 0.03937007874015751446 ) ;
#16295 = CARTESIAN_POINT ( 'NONE',  ( -0.7086614173228346081, 0.000000000000000000, -0.7677165354330708347 ) ) ;
#16296 = FACE_OUTER_BOUND ( 'NONE', #25895, .T. ) ;
#16297 = DIRECTION ( 'NONE',  ( 1.000000000000000000, 0.000000000000000000, 0.000000000000000000 ) ) ;
#16298 = ORIENTED_EDGE ( 'NONE', *, *, #16918, .F. ) ;
#16299 = CARTESIAN_POINT ( 'NONE',  ( 0.3606190329934327310, 0.4297690281277732338, 0.2775610236220472093 ) ) ;
#16300 = ORIENTED_EDGE ( 'NONE', *, *, #26119, .F. ) ;
#16301 = EDGE_CURVE ( 'NONE', #25174, #7018, #7734, .T. ) ;
#16302 = DIRECTION ( 'NONE',  ( 0.000000000000000000, 1.000000000000000000, 0.000000000000000000 ) ) ;
#16303 = CARTESIAN_POINT ( 'NONE',  ( 0.5491102354219981052, -0.3162573801175324051, 0.1061598535667657994 ) ) ;
#16304 = LINE ( 'NONE', #26889, #9625 ) ;
#16305 = CARTESIAN_POINT ( 'NONE',  ( 0.5925575908939920700, -0.2268709785195988371, 0.3929520615588126264 ) ) ;
#16306 = DIRECTION ( 'NONE',  ( 1.000000000000000000, 0.000000000000000000, 0.000000000000000000 ) ) ;
#16307 = CARTESIAN_POINT ( 'NONE',  ( -0.2720459371704843088, 0.3242117229735834716, 0.1377952755905511861 ) ) ;
#16308 = ADVANCED_FACE ( 'NONE', ( #13714 ), #5008, .T. ) ;
#16309 = EDGE_LOOP ( 'NONE', ( #16851, #8525, #3703, #1766 ) ) ;
#16310 = DIRECTION ( 'NONE',  ( 1.000000000000000000, 0.000000000000000000, 0.000000000000000000 ) ) ;
#16311 = CARTESIAN_POINT ( 'NONE',  ( 0.4585215200179055817, -2.840735999735804609E-17, -1.928289503579156516 ) ) ;
#16312 = CARTESIAN_POINT ( 'NONE',  ( 0.6106000000000000316, -1.355930314960630041E-19, 0.000000000000000000 ) ) ;
#16313 = ORIENTED_EDGE ( 'NONE', *, *, #13914, .F. ) ;
#16314 = SURFACE_STYLE_FILL_AREA ( #25339 ) ;
#16315 = CARTESIAN_POINT ( 'NONE',  ( 0.3912931228432222075, -0.3001918266902142696, -1.569881889763779625 ) ) ;
#16316 = EDGE_LOOP ( 'NONE', ( #5292, #18444 ) ) ;
#16317 = CARTESIAN_POINT ( 'NONE',  ( 0.4417361510194462992, 0.05819755867304002989, -1.934055118110236338 ) ) ;
#16318 = EDGE_CURVE ( 'NONE', #5816, #6596, #14919, .T. ) ;
#16319 = EDGE_CURVE ( 'NONE', #17190, #12564, #1353, .T. ) ;
#16320 = AXIS2_PLACEMENT_3D ( 'NONE', #11347, #22505, #1041 ) ;
#16321 = ( LENGTH_UNIT ( ) NAMED_UNIT ( * ) SI_UNIT ( $, .METRE. ) ) ;
#16322 = VERTEX_POINT ( 'NONE', #593 ) ;
#16323 = CARTESIAN_POINT ( 'NONE',  ( -0.4167985568850881561, 0.07349283109919312051, 0.06102165354330708891 ) ) ;
#16324 = DIRECTION ( 'NONE',  ( -0.9659258263664933786, 0.2588190448135666011, 3.169619147893097007E-17 ) ) ;
#16325 = CARTESIAN_POINT ( 'NONE',  ( 0.3855916753051596424, -0.3382184156732262470, 1.747047244094488194 ) ) ;
#16326 = EDGE_LOOP ( 'NONE', ( #21034, #23314, #20911, #25019, #1167, #16333 ) ) ;
#16327 = ORIENTED_EDGE ( 'NONE', *, *, #21317, .F. ) ;
#16328 = CARTESIAN_POINT ( 'NONE',  ( -0.2296683860596777926, -0.2993674444872276297, -3.100567304031764060 ) ) ;
#16329 = CARTESIAN_POINT ( 'NONE',  ( 0.3002886982018046491, -0.1727973894384566000, 0.1377952755905509363 ) ) ;
#16330 = PRODUCT_DEFINITION_SHAPE ( 'NONE', 'NONE',  #10324 ) ;
#16331 = CARTESIAN_POINT ( 'NONE',  ( -0.5375739373539409893, 0.4296723508511055556, 0.1322834645669291320 ) ) ;
#16332 = VERTEX_POINT ( 'NONE', #22194 ) ;
#16333 = ORIENTED_EDGE ( 'NONE', *, *, #4377, .F. ) ;
#16334 = CIRCLE ( 'NONE', #17246, 0.1181102362204724532 ) ;
#16335 = DIRECTION ( 'NONE',  ( 0.000000000000000000, -1.000000000000000000, 0.000000000000000000 ) ) ;
#16336 = DIRECTION ( 'NONE',  ( -1.000000000000000000, 0.000000000000000000, 0.000000000000000000 ) ) ;
#16337 = ORIENTED_EDGE ( 'NONE', *, *, #767, .T. ) ;
#16338 = ORIENTED_EDGE ( 'NONE', *, *, #875, .F. ) ;
#16339 = CARTESIAN_POINT ( 'NONE',  ( -0.7246715730664488042, 0.2518900982766236196, 0.2118286996268641809 ) ) ;
#16340 = CARTESIAN_POINT ( 'NONE',  ( 0.4685039370078740717, 5.737518468446261360E-17, -0.006889763779527558960 ) ) ;
#16341 = EDGE_CURVE ( 'NONE', #4928, #22130, #18268, .T. ) ;
#16342 = AXIS2_PLACEMENT_3D ( 'NONE', #14381, #18579, #5901 ) ;
#16343 = ADVANCED_FACE ( 'NONE', ( #2821 ), #13859, .T. ) ;
#16344 = CARTESIAN_POINT ( 'NONE',  ( -0.1968503937007874127, -0.4724409448818898127, -0.7100240035758484947 ) ) ;
#16345 = CARTESIAN_POINT ( 'NONE',  ( 0.3392387706403788838, 0.1151913129404419922, -3.115157480314960647 ) ) ;
#16346 = CARTESIAN_POINT ( 'NONE',  ( 0.000000000000000000, 0.2952755905511810774, 0.1377952755905511861 ) ) ;
#16347 = CARTESIAN_POINT ( 'NONE',  ( 0.2056553984168021654, 0.2676050456844303316, 1.973425196850393526 ) ) ;
#16348 = CARTESIAN_POINT ( 'NONE',  ( 0.000000000000000000, 0.8661417322803149910, 0.000000000000000000 ) ) ;
#16349 = DIRECTION ( 'NONE',  ( 0.000000000000000000, 0.000000000000000000, 1.000000000000000000 ) ) ;
#16350 = FACE_OUTER_BOUND ( 'NONE', #20942, .T. ) ;
#16351 = DIRECTION ( 'NONE',  ( 0.000000000000000000, 0.000000000000000000, 1.000000000000000000 ) ) ;
#16352 = AXIS2_PLACEMENT_3D ( 'NONE', #7151, #2889, #11115 ) ;
#16353 = VERTEX_POINT ( 'NONE', #5388 ) ;
#16354 = CARTESIAN_POINT ( 'NONE',  ( -0.5382469622847110280, -0.3102483656525752420, 0.2574819594177527593 ) ) ;
#16355 = CONICAL_SURFACE ( 'NONE', #1467, 0.1110236220424516002, 0.7853981642948906217 ) ;
#16356 = CARTESIAN_POINT ( 'NONE',  ( 3.616083068348477634E-17, 0.000000000000000000, 0.2952755905511805778 ) ) ;
#16357 = CARTESIAN_POINT ( 'NONE',  ( 6.147461752294700483E-18, 0.5610236220472440971, 0.07676968503937006694 ) ) ;
#16358 = DIRECTION ( 'NONE',  ( 0.000000000000000000, -1.000000000000000000, 0.000000000000000000 ) ) ;
#16359 = CARTESIAN_POINT ( 'NONE',  ( -0.3242071728275120468, 0.4225965726692976765, 1.747047244094488194 ) ) ;
#16360 = CARTESIAN_POINT ( 'NONE',  ( 0.4856708409200641841, -0.1649135259617057481, 1.766732283464566899 ) ) ;
#16361 = ADVANCED_FACE ( 'NONE', ( #18355 ), #9606, .T. ) ;
#16362 = CIRCLE ( 'NONE', #2799, 0.01181102362204758220 ) ;
#16363 = ORIENTED_EDGE ( 'NONE', *, *, #23404, .T. ) ;
#16364 = CARTESIAN_POINT ( 'NONE',  ( -0.1151913129404333325, 0.3392387706403566239, -3.115157480314960647 ) ) ;
#16365 = ORIENTED_EDGE ( 'NONE', *, *, #24251, .T. ) ;
#16366 = CARTESIAN_POINT ( 'NONE',  ( 0.2118615749922956593, -0.5840192333899354438, 0.09685039370078740717 ) ) ;
#16367 = CARTESIAN_POINT ( 'NONE',  ( 0.7871730179869745880, 0.4038169352867496120, 0.1713250154738354125 ) ) ;
#16368 = CARTESIAN_POINT ( 'NONE',  ( -0.3263749705684267921, -0.1890319631540330891, 0.07637795275590551769 ) ) ;
#16369 = CARTESIAN_POINT ( 'NONE',  ( 0.09590060490395689585, -0.2273032555864669124, 2.185478346456692557E-17 ) ) ;
#16370 = VERTEX_POINT ( 'NONE', #26849 ) ;
#16371 = CARTESIAN_POINT ( 'NONE',  ( 0.4889536969035315761, -0.06441834428467053952, -1.569881889763779625 ) ) ;
#16372 = EDGE_CURVE ( 'NONE', #11528, #17187, #2686, .T. ) ;
#16373 = ADVANCED_FACE ( 'NONE', ( #7092 ), #13572, .T. ) ;
#16374 = ORIENTED_EDGE ( 'NONE', *, *, #17360, .F. ) ;
#16375 = ORIENTED_EDGE ( 'NONE', *, *, #17268, .T. ) ;
#16376 = CIRCLE ( 'NONE', #18583, 1.092519685039370136 ) ;
#16377 = CIRCLE ( 'NONE', #14118, 0.09842519685039370636 ) ;
#16378 = DIRECTION ( 'NONE',  ( 1.000000000000000000, 0.000000000000000000, 0.000000000000000000 ) ) ;
#16379 = DIRECTION ( 'NONE',  ( 0.000000000000000000, -1.000000000000000000, 0.000000000000000000 ) ) ;
#16380 = FACE_OUTER_BOUND ( 'NONE', #7752, .T. ) ;
#16381 = DIRECTION ( 'NONE',  ( 0.000000000000000000, 0.000000000000000000, -1.000000000000000000 ) ) ;
#16382 = CARTESIAN_POINT ( 'NONE',  ( 0.1490609433615242285, 0.000000000000000000, 0.000000000000000000 ) ) ;
#16383 = LINE ( 'NONE', #7914, #22278 ) ;
#16384 = ADVANCED_FACE ( 'NONE', ( #9321 ), #25726, .T. ) ;
#16385 = CARTESIAN_POINT ( 'NONE',  ( -0.6100071611449719988, -0.1652942696472855522, 0.2255770376035045044 ) ) ;
#16386 = CARTESIAN_POINT ( 'NONE',  ( -0.2478439864030017592, 0.4300129863948120579, -1.569881889763779625 ) ) ;
#16387 = VECTOR ( 'NONE', #27840, 39.37007874015748854 ) ;
#16388 = CIRCLE ( 'NONE', #16804, 0.01181102362204754924 ) ;
#16389 = AXIS2_PLACEMENT_3D ( 'NONE', #8498, #200, #23762 ) ;
#16390 = ORIENTED_EDGE ( 'NONE', *, *, #15914, .T. ) ;
#16391 = VERTEX_POINT ( 'NONE', #20213 ) ;
#16392 = AXIS2_PLACEMENT_3D ( 'NONE', #27666, #18751, #16932 ) ;
#16393 = EDGE_CURVE ( 'NONE', #26363, #8023, #7212, .T. ) ;
#16394 = ORIENTED_EDGE ( 'NONE', *, *, #4506, .F. ) ;
#16395 = DIRECTION ( 'NONE',  ( -0.9396926207859082059, -0.3420201433256689905, 0.000000000000000000 ) ) ;
#16396 = ADVANCED_FACE ( 'NONE', ( #11738 ), #27421, .T. ) ;
#16397 = CARTESIAN_POINT ( 'NONE',  ( -0.7874015748031496509, 5.862181872755905604E-06, -1.869015748010449007 ) ) ;
#16398 = CIRCLE ( 'NONE', #4233, 0.5007874015748031704 ) ;
#16399 = CARTESIAN_POINT ( 'NONE',  ( 0.07669076177803835215, 0.1968503937007873850, -3.568838416488088860 ) ) ;
#16400 = ORIENTED_EDGE ( 'NONE', *, *, #19037, .T. ) ;
#16401 = DIRECTION ( 'NONE',  ( 1.000000000000000000, 0.000000000000000000, 0.000000000000000000 ) ) ;
#16402 = VERTEX_POINT ( 'NONE', #27281 ) ;
#16403 = SURFACE_SIDE_STYLE ('',( #1851 ) ) ;
#16404 = CARTESIAN_POINT ( 'NONE',  ( 0.3937007873768824662, 0.000000000000000000, 2.090519358671640647E-11 ) ) ;
#16405 = CLOSED_SHELL ( 'NONE', ( #25676, #6629, #3592, #9258, #154, #26630, #7259, #13259 ) ) ;
#16406 = CARTESIAN_POINT ( 'NONE',  ( -0.1709077104829875848, -0.4707213777573787672, 0.2574819596263889787 ) ) ;
#16407 = CARTESIAN_POINT ( 'NONE',  ( -0.03937007874015747977, -0.6299212598425196763, 7.714310545810098438E-17 ) ) ;
#16408 = CARTESIAN_POINT ( 'NONE',  ( -0.4069448477569433953, -0.3121994997578269593, -1.550196850393700920 ) ) ;
#16409 = DIRECTION ( 'NONE',  ( 0.000000000000000000, -1.000000000000000000, 0.000000000000000000 ) ) ;
#16410 = CARTESIAN_POINT ( 'NONE',  ( -0.1291602287245499914, -0.3543605079199910191, 0.1992150590373740204 ) ) ;
#16411 = B_SPLINE_CURVE_WITH_KNOTS ( 'NONE', 3,
 ( #9962, #15907, #7568, #3030, #27073, #18564 ),
 .UNSPECIFIED., .F., .F.,
 ( 4, 2, 4 ),
 ( 0.6902184472752670441, 0.6915327610580710438, 0.6928470748408740443 ),
 .UNSPECIFIED. ) ;
#16412 = CARTESIAN_POINT ( 'NONE',  ( -0.07214854559198564943, -0.5476281405333169872, 0.9202755905511811330 ) ) ;
#16413 = DIRECTION ( 'NONE',  ( 0.000000000000000000, 0.000000000000000000, 1.000000000000000000 ) ) ;
#16414 = AXIS2_PLACEMENT_3D ( 'NONE', #3652, #16810, #20903 ) ;
#16415 = DIRECTION ( 'NONE',  ( 7.017815000000000124E-18, -1.000000000000000000, 0.000000000000000000 ) ) ;
#16416 = EDGE_LOOP ( 'NONE', ( #6168, #19443, #17867, #6339, #20325 ) ) ;
#16417 = CARTESIAN_POINT ( 'NONE',  ( -0.4162944719209866196, 0.3316996361851582975, 0.3401599409343964431 ) ) ;
#16418 = EDGE_CURVE ( 'NONE', #16265, #1951, #17154, .T. ) ;
#16419 = CARTESIAN_POINT ( 'NONE',  ( 0.4889536969035315761, -0.06441834428467053952, -1.569881889763779625 ) ) ;
#16420 = CARTESIAN_POINT ( 'NONE',  ( 0.000000000000000000, 0.000000000000000000, 0.1771653543307086520 ) ) ;
#16421 = DIRECTION ( 'NONE',  ( -0.000000000000000000, -1.000000000000000000, -0.000000000000000000 ) ) ;
#16422 = DIRECTION ( 'NONE',  ( 1.224646799147353207E-16, 1.000000000000000000, -0.000000000000000000 ) ) ;
#16423 = EDGE_CURVE ( 'NONE', #11982, #13935, #23348, .T. ) ;
#16424 = ORIENTED_EDGE ( 'NONE', *, *, #9138, .T. ) ;
#16425 = VERTEX_POINT ( 'NONE', #3672 ) ;
#16426 = CARTESIAN_POINT ( 'NONE',  ( -0.05981201256803149457, 1.563633646945708833, 1.633858267716535639 ) ) ;
#16427 = CARTESIAN_POINT ( 'NONE',  ( 0.03008364706454716778, 0.2273032555864669124, 0.000000000000000000 ) ) ;
#16428 = LINE ( 'NONE', #12327, #15548 ) ;
#16429 = CARTESIAN_POINT ( 'NONE',  ( -0.5511811023622047445, 0.000000000000000000, 0.000000000000000000 ) ) ;
#16430 = VERTEX_POINT ( 'NONE', #9900 ) ;
#16431 = CARTESIAN_POINT ( 'NONE',  ( -0.0007756954652713807415, 0.7174612052785541705, 0.3122824329337317018 ) ) ;
#16432 = VERTEX_POINT ( 'NONE', #8212 ) ;
#16433 = VECTOR ( 'NONE', #27442, 39.37007874015748143 ) ;
#16434 = CARTESIAN_POINT ( 'NONE',  ( 0.000000000000000000, 0.07874015748031495954, 1.988188976307287970 ) ) ;
#16435 = CARTESIAN_POINT ( 'NONE',  ( -0.4848217985909654137, 0.000000000000000000, -0.04133858267716535029 ) ) ;
#16436 = CARTESIAN_POINT ( 'NONE',  ( -0.1968503937007874127, -3.496765354330708585E-17, -0.09092130223458683158 ) ) ;
#16437 = AXIS2_PLACEMENT_3D ( 'NONE', #3553, #21087, #14320 ) ;
#16438 = CARTESIAN_POINT ( 'NONE',  ( 0.3714054139060134485, 0.06566393819133227450, 0.07637549214372835182 ) ) ;
#16439 = DIRECTION ( 'NONE',  ( 0.000000000000000000, 0.000000000000000000, -1.000000000000000000 ) ) ;
#16440 = CARTESIAN_POINT ( 'NONE',  ( 0.6882266799383700562, -0.2663285262597259728, -0.2694682288251842861 ) ) ;
#16441 = EDGE_LOOP ( 'NONE', ( #25538, #18517, #980, #13375 ) ) ;
#16442 = EDGE_CURVE ( 'NONE', #804, #15069, #16706, .T. ) ;
#16443 = SURFACE_STYLE_FILL_AREA ( #16576 ) ;
#16444 = DIRECTION ( 'NONE',  ( 0.000000000000000000, 0.000000000000000000, 1.000000000000000000 ) ) ;
#16445 = FACE_OUTER_BOUND ( 'NONE', #25831, .T. ) ;
#16446 = CARTESIAN_POINT ( 'NONE',  ( -0.2842139414039350775, -0.2181198385717931787, -3.115157480314961091 ) ) ;
#16447 = CARTESIAN_POINT ( 'NONE',  ( -0.0006679551606482677165, 0.5322830454629158270, 0.1322834645669291320 ) ) ;
#16448 = CIRCLE ( 'NONE', #24111, 0.5007874015748031704 ) ;
#16449 = ORIENTED_EDGE ( 'NONE', *, *, #15730, .T. ) ;
#16450 = CARTESIAN_POINT ( 'NONE',  ( 0.3349573549949902418, -0.2938049579018460755, -1.934055118110236338 ) ) ;
#16451 = AXIS2_PLACEMENT_3D ( 'NONE', #6092, #12841, #20908 ) ;
#16452 = ORIENTED_EDGE ( 'NONE', *, *, #10864, .T. ) ;
#16453 = VERTEX_POINT ( 'NONE', #16833 ) ;
#16454 = ADVANCED_FACE ( 'NONE', ( #12025 ), #4530, .T. ) ;
#16455 = VERTEX_POINT ( 'NONE', #20640 ) ;
#16456 = AXIS2_PLACEMENT_3D ( 'NONE', #10044, #12306, #20931 ) ;
#16457 = CARTESIAN_POINT ( 'NONE',  ( -0.4609540795476803621, -0.4491800479312370031, -0.3703714726251385869 ) ) ;
#16458 = CARTESIAN_POINT ( 'NONE',  ( 0.3121994997598398491, -0.4069448477555819843, 1.747047244094488194 ) ) ;
#16459 = EDGE_CURVE ( 'NONE', #5280, #14016, #20759, .T. ) ;
#16460 = ORIENTED_EDGE ( 'NONE', *, *, #9380, .T. ) ;
#16461 = VERTEX_POINT ( 'NONE', #21207 ) ;
#16462 = CARTESIAN_POINT ( 'NONE',  ( -0.2296683860596825943, 0.2993674444872254092, -3.100567304031761395 ) ) ;
#16463 = CARTESIAN_POINT ( 'NONE',  ( -0.09842519685039370636, 0.2165354330708661457, -3.272637795275590733 ) ) ;
#16464 = ADVANCED_FACE ( 'NONE', ( #7931, #1290 ), #19075, .T. ) ;
#16465 = VECTOR ( 'NONE', #10261, 39.37007874015748143 ) ;
#16466 = ORIENTED_EDGE ( 'NONE', *, *, #7162, .T. ) ;
#16467 = VERTEX_POINT ( 'NONE', #14444 ) ;
#16468 = CARTESIAN_POINT ( 'NONE',  ( -0.3573825339541266133, -0.7156596623968717319, -0.6596724844134214116 ) ) ;
#16469 = DIRECTION ( 'NONE',  ( 0.000000000000000000, -0.9984511807834833830, -0.05563487747868002542 ) ) ;
#16470 = ORIENTED_EDGE ( 'NONE', *, *, #11166, .T. ) ;
#16471 = ORIENTED_EDGE ( 'NONE', *, *, #21994, .F. ) ;
#16472 = VERTEX_POINT ( 'NONE', #3973 ) ;
#16473 = DIRECTION ( 'NONE',  ( 0.1736481776669309418, 0.9848077530122079093, 0.000000000000000000 ) ) ;
#16474 = DIRECTION ( 'NONE',  ( 0.000000000000000000, 1.000000000000000000, 0.000000000000000000 ) ) ;
#16475 = EDGE_CURVE ( 'NONE', #285, #16188, #20306, .T. ) ;
#16476 = CARTESIAN_POINT ( 'NONE',  ( -0.1151913129404409791, -0.3392387706403589553, -3.115157480314960647 ) ) ;
#16477 = CIRCLE ( 'NONE', #4302, 0.07910393700787400617 ) ;
#16478 = DIRECTION ( 'NONE',  ( -0.7818314824680295816, 0.6234898018587339275, 0.000000000000000000 ) ) ;
#16479 = CARTESIAN_POINT ( 'NONE',  ( -0.2676050456844304981, 0.2056553984168023042, 1.973425196850394858 ) ) ;
#16480 = CARTESIAN_POINT ( 'NONE',  ( -0.3040421205569480145, 1.249037478091203024, -0.7140903627573721435 ) ) ;
#16481 = CARTESIAN_POINT ( 'NONE',  ( -0.4842519685039370358, 0.000000000000000000, -0.1309055118110236116 ) ) ;
#16482 = CARTESIAN_POINT ( 'NONE',  ( 0.000000000000000000, 0.000000000000000000, 0.07637795275590551769 ) ) ;
#16483 = AXIS2_PLACEMENT_3D ( 'NONE', #21956, #15342, #17427 ) ;
#16484 = ORIENTED_EDGE ( 'NONE', *, *, #13842, .T. ) ;
#16485 = CARTESIAN_POINT ( 'NONE',  ( -0.0005696707463070112927, 0.4606295689977898400, 0.1771653543307085965 ) ) ;
#16486 = EDGE_CURVE ( 'NONE', #11391, #22315, #22342, .T. ) ;
#16487 = CARTESIAN_POINT ( 'NONE',  ( 0.4771018889076559244, 0.3804760601893846794, 0.3661437007874016047 ) ) ;
#16488 = DIRECTION ( 'NONE',  ( -0.9790454724845842893, 0.1018208755700880375, -0.1763589297585410332 ) ) ;
#16489 = ORIENTED_EDGE ( 'NONE', *, *, #27381, .T. ) ;
#16490 = CARTESIAN_POINT ( 'NONE',  ( 0.09586345242798374744, 0.2165354330708660902, -3.573990933499927802 ) ) ;
#16491 = EDGE_CURVE ( 'NONE', #16425, #19868, #20813, .T. ) ;
#16492 = ORIENTED_EDGE ( 'NONE', *, *, #2812, .F. ) ;
#16493 = ADVANCED_FACE ( 'NONE', ( #20921 ), #27547, .F. ) ;
#16494 = DIRECTION ( 'NONE',  ( -1.000000000000000000, 0.000000000000000000, 0.000000000000000000 ) ) ;
#16495 = ORIENTED_EDGE ( 'NONE', *, *, #10718, .T. ) ;
#16496 = CARTESIAN_POINT ( 'NONE',  ( -0.7874015748031496509, 0.4828108945773819105, 0.1423708153504031348 ) ) ;
#16497 = CARTESIAN_POINT ( 'NONE',  ( 0.1517511419331917244, -0.4888569460008191370, 0.05146517564439353348 ) ) ;
#16498 = CARTESIAN_POINT ( 'NONE',  ( 0.6102362204724409711, 0.000000000000000000, 0.2362204724409449064 ) ) ;
#16499 = VERTEX_POINT ( 'NONE', #16530 ) ;
#16500 = VERTEX_POINT ( 'NONE', #23195 ) ;
#16501 = AXIS2_PLACEMENT_3D ( 'NONE', #6710, #13461, #19279 ) ;
#16502 = CARTESIAN_POINT ( 'NONE',  ( 0.4921259842519685179, 0.03220957031754003580, -1.550196850393700920 ) ) ;
#16503 = VERTEX_POINT ( 'NONE', #3826 ) ;
#16504 = ORIENTED_EDGE ( 'NONE', *, *, #6553, .F. ) ;
#16505 = AXIS2_PLACEMENT_3D ( 'NONE', #6252, #2139, #10757 ) ;
#16506 = DIMENSIONAL_EXPONENTS ( 1.000000000000000000, 0.000000000000000000, 0.000000000000000000, 0.000000000000000000, 0.000000000000000000, 0.000000000000000000, 0.000000000000000000 ) ;
#16507 = CONTEXT_DEPENDENT_SHAPE_REPRESENTATION ( #11244, #6899 ) ;
#16508 = LINE ( 'NONE', #16798, #9021 ) ;
#16509 = CARTESIAN_POINT ( 'NONE',  ( 0.1516263115863346334, 0.1971492568089271424, -0.4530651079966795947 ) ) ;
#16510 = DIRECTION ( 'NONE',  ( 1.000000000000000000, 0.000000000000000000, 0.000000000000000000 ) ) ;
#16511 = VERTEX_POINT ( 'NONE', #8760 ) ;
#16512 = CYLINDRICAL_SURFACE ( 'NONE', #611, 0.06200787401574805319 ) ;
#16513 = AXIS2_PLACEMENT_3D ( 'NONE', #16525, #23190, #14147 ) ;
#16514 = DIRECTION ( 'NONE',  ( -1.000000000000000000, 0.000000000000000000, 0.000000000000000000 ) ) ;
#16515 = CARTESIAN_POINT ( 'NONE',  ( 0.3722026523000413478, 4.558167867734008572E-17, -0.05511811023622047168 ) ) ;
#16516 = DIRECTION ( 'NONE',  ( -0.7071067811865470176, -0.7071067811865480168, 0.000000000000000000 ) ) ;
#16517 = CARTESIAN_POINT ( 'NONE',  ( -0.6062104012196082303, -0.1785888610321556547, 0.2237894313402810087 ) ) ;
#16518 = DIRECTION ( 'NONE',  ( -0.000000000000000000, -1.000000000000000000, -0.000000000000000000 ) ) ;
#16519 = CARTESIAN_POINT ( 'NONE',  ( 0.000000000000000000, 0.07874015748031508444, 0.000000000000000000 ) ) ;
#16520 = PLANE ( 'NONE',  #2452 ) ;
#16521 = EDGE_LOOP ( 'NONE', ( #7495, #19360, #8968, #5736 ) ) ;
#16522 = EDGE_LOOP ( 'NONE', ( #27282, #15466, #4210, #17666, #5160, #15514 ) ) ;
#16523 = ORIENTED_EDGE ( 'NONE', *, *, #16948, .F. ) ;
#16524 = AXIS2_PLACEMENT_3D ( 'NONE', #27791, #71, #4800 ) ;
#16525 = CARTESIAN_POINT ( 'NONE',  ( 0.000000000000000000, 0.000000000000000000, -0.1377952755905511861 ) ) ;
#16526 = AXIS2_PLACEMENT_3D ( 'NONE', #26197, #15483, #21967 ) ;
#16527 = DIRECTION ( 'NONE',  ( 0.000000000000000000, 1.000000000000000000, 0.000000000000000000 ) ) ;
#16528 = FACE_OUTER_BOUND ( 'NONE', #10371, .T. ) ;
#16529 = CARTESIAN_POINT ( 'NONE',  ( 0.3198827364362346048, 3.917433692791311553E-17, -0.1725236688546921415 ) ) ;
#16530 = CARTESIAN_POINT ( 'NONE',  ( 0.3976891862754212137, 0.7181140751201200434, -0.6642661073933326943 ) ) ;
#16531 = ORIENTED_EDGE ( 'NONE', *, *, #14629, .T. ) ;
#16532 = AXIS2_PLACEMENT_3D ( 'NONE', #693, #13536, #8888 ) ;
#16533 = FACE_BOUND ( 'NONE', #13894, .T. ) ;
#16534 = CARTESIAN_POINT ( 'NONE',  ( -0.0005896702191535062526, 0.4865884552403880736, 0.1827409795202798448 ) ) ;
#16535 = CARTESIAN_POINT ( 'NONE',  ( -0.2104048168856049172, -0.4354435989245551419, 0.2715646632391802151 ) ) ;
#16536 = EDGE_CURVE ( 'NONE', #25553, #333, #8638, .T. ) ;
#16537 = EDGE_CURVE ( 'NONE', #14962, #13935, #11275, .T. ) ;
#16538 = DIRECTION ( 'NONE',  ( -1.000000000000000000, 0.000000000000000000, 0.000000000000000000 ) ) ;
#16539 = VERTEX_POINT ( 'NONE', #6656 ) ;
#16540 = CARTESIAN_POINT ( 'NONE',  ( 0.7872492282968406307, 0.2535447773504393987, -0.2765860549081538555 ) ) ;
#16541 = PRODUCT_DEFINITION ( 'UNKNOWN', '', #15637, #100 ) ;
#16542 = EDGE_LOOP ( 'NONE', ( #1890, #27380, #27772, #8104 ) ) ;
#16543 = CARTESIAN_POINT ( 'NONE',  ( -0.3661417322834645272, -0.4724409448818898127, -0.8182917201112815953 ) ) ;
#16544 = EDGE_CURVE ( 'NONE', #11010, #240, #25781, .T. ) ;
#16545 = DIRECTION ( 'NONE',  ( 0.000000000000000000, 0.000000000000000000, 1.000000000000000000 ) ) ;
#16546 = ( LENGTH_UNIT ( ) NAMED_UNIT ( * ) SI_UNIT ( $, .METRE. ) ) ;
#16547 = CARTESIAN_POINT ( 'NONE',  ( -0.5230301363771188150, -0.1775991818008711975, 0.9399606299212598381 ) ) ;
#16548 = EDGE_CURVE ( 'NONE', #4474, #26390, #6371, .T. ) ;
#16549 = CIRCLE ( 'NONE', #5741, 0.1181102362204720091 ) ;
#16550 = EDGE_CURVE ( 'NONE', #18664, #24074, #15281, .T. ) ;
#16551 = DIRECTION ( 'NONE',  ( 1.000000000000000000, 0.000000000000000000, 0.000000000000000000 ) ) ;
#16552 = ORIENTED_EDGE ( 'NONE', *, *, #21093, .T. ) ;
#16553 = PRODUCT ( 'ISO 4762 M5x16 Socket Head Cap Screw', 'ISO 4762 M5x16 Socket Head Cap Screw', '', ( #2873 ) ) ;
#16554 = CARTESIAN_POINT ( 'NONE',  ( 0.000000000000000000, 0.000000000000000000, -4.097771653543307347E-17 ) ) ;
#16555 = EDGE_LOOP ( 'NONE', ( #26358, #2697, #14315, #1650 ) ) ;
#16556 = ( GEOMETRIC_REPRESENTATION_CONTEXT ( 3 ) GLOBAL_UNCERTAINTY_ASSIGNED_CONTEXT ( ( #25134 ) ) GLOBAL_UNIT_ASSIGNED_CONTEXT ( ( #14651, #7992, #10226 ) ) REPRESENTATION_CONTEXT ( 'NONE', 'WORKASPACE' ) ) ;
#16557 = CARTESIAN_POINT ( 'NONE',  ( 0.4004922687719589258, 0.3511586785140410893, 1.747047244094488416 ) ) ;
#16558 = ORIENTED_EDGE ( 'NONE', *, *, #23544, .F. ) ;
#16559 = EDGE_LOOP ( 'NONE', ( #6915, #347 ) ) ;
#16560 = DIRECTION ( 'NONE',  ( 1.000000000000000078E-15, -1.000000000000000000, 0.000000000000000000 ) ) ;
#16561 = CARTESIAN_POINT ( 'NONE',  ( 0.000000000000000000, 0.000000000000000000, -0.4724409448818898127 ) ) ;
#16562 = DIRECTION ( 'NONE',  ( 0.000000000000000000, 0.000000000000000000, -1.000000000000000000 ) ) ;
#16563 = CARTESIAN_POINT ( 'NONE',  ( 0.000000000000000000, 0.000000000000000000, 2.504921259842519898 ) ) ;
#16564 = VERTEX_POINT ( 'NONE', #23484 ) ;
#16565 = CARTESIAN_POINT ( 'NONE',  ( -0.5704973819974966665, -0.5016125552370697127, 0.9930863283245008333 ) ) ;
#16566 = EDGE_LOOP ( 'NONE', ( #13406, #20775, #1050, #11512, #387, #16009 ) ) ;
#16567 = ORIENTED_EDGE ( 'NONE', *, *, #11690, .T. ) ;
#16568 = CARTESIAN_POINT ( 'NONE',  ( -0.3661417322834645272, -0.4724409448818898127, 0.8182917201112815953 ) ) ;
#16569 = DIRECTION ( 'NONE',  ( 0.8660254037844387076, 0.4999999999999998890, -0.000000000000000000 ) ) ;
#16570 = ( GEOMETRIC_REPRESENTATION_CONTEXT ( 3 ) GLOBAL_UNCERTAINTY_ASSIGNED_CONTEXT ( ( #23243 ) ) GLOBAL_UNIT_ASSIGNED_CONTEXT ( ( #25683, #10552, #10700 ) ) REPRESENTATION_CONTEXT ( 'NONE', 'WORKASPACE' ) ) ;
#16571 = STYLED_ITEM ( 'NONE', ( #23094 ), #3022 ) ;
#16572 = CARTESIAN_POINT ( 'NONE',  ( 0.000000000000000000, 0.000000000000000000, -0.07578740157480315376 ) ) ;
#16573 = CARTESIAN_POINT ( 'NONE',  ( -0.3529960615001250801, 0.06172929298804197967, 0.09506557084278018099 ) ) ;
#16574 = CARTESIAN_POINT ( 'NONE',  ( 0.5890517850735842442, -0.1589264097367456829, -0.07874015748031495954 ) ) ;
#16575 = ORIENTED_EDGE ( 'NONE', *, *, #18802, .F. ) ;
#16576 = FILL_AREA_STYLE ('',( #16876 ) ) ;
#16577 = FACE_BOUND ( 'NONE', #26121, .T. ) ;
#16578 = EDGE_CURVE ( 'NONE', #3390, #12667, #15307, .T. ) ;
#16579 = CIRCLE ( 'NONE', #4413, 0.8267716535433071723 ) ;
#16580 = FACE_OUTER_BOUND ( 'NONE', #10190, .T. ) ;
#16581 = EDGE_CURVE ( 'NONE', #21208, #19384, #6328, .T. ) ;
#16582 = ORIENTED_EDGE ( 'NONE', *, *, #13872, .F. ) ;
#16583 = CARTESIAN_POINT ( 'NONE',  ( -0.2693781226335786316, -0.2362017869179856566, -3.115157480314961980 ) ) ;
#16584 = CARTESIAN_POINT ( 'NONE',  ( 0.3252100150720381722, -0.3707612262533039327, -1.569881889763779625 ) ) ;
#16585 = EDGE_CURVE ( 'NONE', #21933, #18631, #19401, .T. ) ;
#16586 = B_SPLINE_CURVE_WITH_KNOTS ( 'NONE', 3,
 ( #10346, #5708, #16713, #14768, #23511, #25178 ),
 .UNSPECIFIED., .F., .F.,
 ( 4, 2, 4 ),
 ( 0.000000000000000000, 0.2500000000000000000, 0.5000000000000000000 ),
 .UNSPECIFIED. ) ;
#16587 = ORIENTED_EDGE ( 'NONE', *, *, #2422, .F. ) ;
#16588 = CARTESIAN_POINT ( 'NONE',  ( 0.05819755867303724045, 0.4417361510194101615, -1.934055118110236338 ) ) ;
#16589 = EDGE_CURVE ( 'NONE', #1934, #147, #19647, .T. ) ;
#16590 = ORIENTED_EDGE ( 'NONE', *, *, #20313, .T. ) ;
#16591 = ORIENTED_EDGE ( 'NONE', *, *, #10114, .T. ) ;
#16592 = ORIENTED_EDGE ( 'NONE', *, *, #15699, .F. ) ;
#16593 = AXIS2_PLACEMENT_3D ( 'NONE', #24669, #20268, #5141 ) ;
#16594 = CARTESIAN_POINT ( 'NONE',  ( -0.5743180011325290657, -0.1838911706806881652, -0.2570840403994941181 ) ) ;
#16595 = SHAPE_DEFINITION_REPRESENTATION ( #5079, #4612 ) ;
#16596 = CARTESIAN_POINT ( 'NONE',  ( 0.4777261797697469614, 0.2355331214654221850, 1.747047244094488194 ) ) ;
#16597 = ORIENTED_EDGE ( 'NONE', *, *, #25911, .F. ) ;
#16598 = DIRECTION ( 'NONE',  ( 0.000000000000000000, 0.000000000000000000, 1.000000000000000000 ) ) ;
#16599 = ORIENTED_EDGE ( 'NONE', *, *, #21466, .T. ) ;
#16600 = CYLINDRICAL_SURFACE ( 'NONE', #1149, 0.06200787401574775481 ) ;
#16601 = PLANE ( 'NONE',  #13333 ) ;
#16602 = CARTESIAN_POINT ( 'NONE',  ( -0.2070393714800602414, -0.08522740305600375044, -0.07874015748031495954 ) ) ;
#16603 = CARTESIAN_POINT ( 'NONE',  ( 0.04638120790932896698, -0.3520466617656974884, 1.953740157480315043 ) ) ;
#16604 = EDGE_LOOP ( 'NONE', ( #15578, #9829, #23589, #785, #15574, #23861, #22780 ) ) ;
#16605 = CARTESIAN_POINT ( 'NONE',  ( -0.5905726622054751074, -0.1477137071932877743, -0.2496838636049826254 ) ) ;
#16606 = DIRECTION ( 'NONE',  ( 1.000000000000000000, 0.000000000000000000, 0.000000000000000000 ) ) ;
#16608 = CARTESIAN_POINT ( 'NONE',  ( 0.5476281405333121022, -0.07214854559198019546, 0.9399606299212598381 ) ) ;
#16607 = CARTESIAN_POINT ( 'NONE',  ( -0.1896185148830506761, -0.3289909311256231095, -3.100567304031762728 ) ) ;
#16609 = VERTEX_POINT ( 'NONE', #23617 ) ;
#16610 = VERTEX_POINT ( 'NONE', #2256 ) ;
#16611 = DIRECTION ( 'NONE',  ( 0.000000000000000000, 0.000000000000000000, -1.000000000000000000 ) ) ;
#16612 = CARTESIAN_POINT ( 'NONE',  ( 0.1490609433576163545, -0.2393035190829114200, 0.4144858534816307505 ) ) ;
#16613 = VECTOR ( 'NONE', #7196, 39.37007874015748143 ) ;
#16614 = EDGE_CURVE ( 'NONE', #5599, #26227, #7881, .T. ) ;
#16615 = TOROIDAL_SURFACE ( 'NONE', #26983, 0.5610236220472440971, 0.1003937007874015908 ) ;
#16616 = CARTESIAN_POINT ( 'NONE',  ( -0.2693339498142315880, 0.2362439534887433579, -3.115157480314960647 ) ) ;
#16617 = CARTESIAN_POINT ( 'NONE',  ( 0.1490609433615240342, 0.2393035190771456711, 0.4144858534716441278 ) ) ;
#16618 = COLOUR_RGB ( '', 0.40784314, 0.44705882, 0.49803922) ;
#16619 = CARTESIAN_POINT ( 'NONE',  ( 0.2997912780622382090, -0.1736589463928937538, 0.1377952755905513249 ) ) ;
#16620 = CARTESIAN_POINT ( 'NONE',  ( -0.3334645669291338987, 0.8151331854455394765, -1.007197927683596506 ) ) ;
#16621 = EDGE_CURVE ( 'NONE', #15134, #3577, #11725, .T. ) ;
#16622 = DIRECTION ( 'NONE',  ( 0.000000000000000000, 1.000000000000000000, 0.000000000000000000 ) ) ;
#16623 = CARTESIAN_POINT ( 'NONE',  ( 0.3073078020566822888, 0.3671449284701643889, 0.08349695147736714562 ) ) ;
#16625 = FACE_OUTER_BOUND ( 'NONE', #15673, .T. ) ;
#16624 = AXIS2_PLACEMENT_3D ( 'NONE', #2688, #18208, #11875 ) ;
#16626 = ADVANCED_FACE ( 'NONE', ( #8623, #10880 ), #17105, .T. ) ;
#16627 = ORIENTED_EDGE ( 'NONE', *, *, #8131, .T. ) ;
#16628 = FACE_OUTER_BOUND ( 'NONE', #9749, .T. ) ;
#16629 = DIRECTION ( 'NONE',  ( -1.000000000000000000, 0.000000000000000000, 0.000000000000000000 ) ) ;
#16630 = CARTESIAN_POINT ( 'NONE',  ( 0.000000000000000000, 0.000000000000000000, 0.1377952755905511861 ) ) ;
#16631 = PLANE ( 'NONE',  #10316 ) ;
#16632 = CARTESIAN_POINT ( 'NONE',  ( -0.3263749705684267921, -0.1890319631540330891, 0.07637795275590551769 ) ) ;
#16633 = SPHERICAL_SURFACE ( 'NONE', #17798, 0.1003956692913385851 ) ;
#16634 = CARTESIAN_POINT ( 'NONE',  ( 0.06048688188729493126, 0.2165354330708660902, -3.626935712834465697 ) ) ;
#16635 = DIRECTION ( 'NONE',  ( 1.000000000000000000, 0.000000000000000000, 0.000000000000000000 ) ) ;
#16636 = CARTESIAN_POINT ( 'NONE',  ( -0.2173565190932491564, -0.5952284643155388855, 0.1061598535666244958 ) ) ;
#16637 = CARTESIAN_POINT ( 'NONE',  ( 0.2564944395515434961, -0.4441657790107952364, 1.766732283464566899 ) ) ;
#16638 = TOROIDAL_SURFACE ( 'NONE', #3996, 0.4986013261500205074, 0.02755905511811023584 ) ;
#16639 = EDGE_CURVE ( 'NONE', #9956, #19035, #26595, .T. ) ;
#16640 = EDGE_LOOP ( 'NONE', ( #19311, #8581, #15645, #25210 ) ) ;
#16641 = ORIENTED_EDGE ( 'NONE', *, *, #2816, .T. ) ;
#16642 = AXIS2_PLACEMENT_3D ( 'NONE', #22045, #22321, #11308 ) ;
#16643 = CARTESIAN_POINT ( 'NONE',  ( -0.2693339498142315880, 0.2362439534887433579, -3.115157480314960647 ) ) ;
#16644 = EDGE_LOOP ( 'NONE', ( #1698, #18489, #2248, #3929, #21178, #23298, #5787, #14182 ) ) ;
#16645 = VECTOR ( 'NONE', #13662, 39.37007874015748143 ) ;
#16646 = CARTESIAN_POINT ( 'NONE',  ( 0.4790450267257945760, 0.08506312950213980317, 0.2467937633157138710 ) ) ;
#16647 = CARTESIAN_POINT ( 'NONE',  ( -0.0004974201395671521515, 0.3464563358313494934, 0.1377952755905512139 ) ) ;
#16648 = B_SPLINE_CURVE_WITH_KNOTS ( 'NONE', 3,
 ( #5598, #9031, #18289, #27214 ),
 .UNSPECIFIED., .F., .F.,
 ( 4, 4 ),
 ( 1.162880698919837918, 1.164573402063411978 ),
 .UNSPECIFIED. ) ;
#16649 = CARTESIAN_POINT ( 'NONE',  ( 0.3346456692913385988, 0.02190250779246873461, 1.953740157480315043 ) ) ;
#16650 = EDGE_LOOP ( 'NONE', ( #9279, #9916, #2024, #4778, #18313 ) ) ;
#16651 = ORIENTED_EDGE ( 'NONE', *, *, #21682, .T. ) ;
#16652 = CARTESIAN_POINT ( 'NONE',  ( -0.1585706980422225409, -0.4669911931914833558, -1.550196850393700920 ) ) ;
#16653 = FACE_BOUND ( 'NONE', #20225, .T. ) ;
#16654 = AXIS2_PLACEMENT_3D ( 'NONE', #6717, #13467, #12920 ) ;
#16655 = ORIENTED_EDGE ( 'NONE', *, *, #9048, .T. ) ;
#16656 = ORIENTED_EDGE ( 'NONE', *, *, #8429, .T. ) ;
#16657 = VERTEX_POINT ( 'NONE', #4114 ) ;
#16658 = EDGE_CURVE ( 'NONE', #6454, #20576, #6319, .T. ) ;
#16659 = CARTESIAN_POINT ( 'NONE',  ( 0.000000000000000000, 0.000000000000000000, 0.2362204724409449064 ) ) ;
#16660 = CARTESIAN_POINT ( 'NONE',  ( 0.2118615749922956593, -0.5840192333899354438, 0.09685039370078740717 ) ) ;
#16661 = FACE_OUTER_BOUND ( 'NONE', #12163, .T. ) ;
#16662 = DIRECTION ( 'NONE',  ( 1.000000000000000000, 0.000000000000000000, 0.000000000000000000 ) ) ;
#16663 = EDGE_CURVE ( 'NONE', #21686, #23531, #25025, .T. ) ;
#16664 = AXIS2_PLACEMENT_3D ( 'NONE', #1363, #9975, #8152 ) ;
#16665 = CIRCLE ( 'NONE', #15337, 0.07677165354330708902 ) ;
#16666 = ORIENTED_EDGE ( 'NONE', *, *, #3654, .F. ) ;
#16667 = CARTESIAN_POINT ( 'NONE',  ( -0.5840204509605140260, -0.4658379333985104287, 0.9954608945792949859 ) ) ;
#16668 = CIRCLE ( 'NONE', #16156, 0.09143349766193348271 ) ;
#16669 = CARTESIAN_POINT ( 'NONE',  ( -0.5905511811023621549, 1.087444635826771533, -0.1051828227901525498 ) ) ;
#16670 = CARTESIAN_POINT ( 'NONE',  ( 0.03008364706454716778, -0.1136516277932334562, 0.1968503937007874127 ) ) ;
#16671 = CARTESIAN_POINT ( 'NONE',  ( 0.9842519685039370358, -2.559055118110236560, 0.2952755905511810774 ) ) ;
#16672 = CARTESIAN_POINT ( 'NONE',  ( -0.6019536057979716359, -0.1934596109017840404, 0.2216182498624969244 ) ) ;
#16673 = DIRECTION ( 'NONE',  ( -0.9790454724845842893, 0.1018208755700880375, -0.1763589297585410332 ) ) ;
#16674 = CIRCLE ( 'NONE', #9884, 0.4807043897637795493 ) ;
#16675 = CARTESIAN_POINT ( 'NONE',  ( -0.4858607088160732390, -0.2805118110236220486, 0.1771653543307086520 ) ) ;
#16676 = CARTESIAN_POINT ( 'NONE',  ( 0.5905511811023621549, 0.000000000000000000, 0.9399606299212598381 ) ) ;
#16677 = B_SPLINE_CURVE_WITH_KNOTS ( 'NONE', 3,
 ( #8601, #6769, #7037, #19893, #168, #15531 ),
 .UNSPECIFIED., .F., .F.,
 ( 4, 2, 4 ),
 ( 0.3108507187342960387, 0.3125269569790680158, 0.3142031952238389936 ),
 .UNSPECIFIED. ) ;
#16678 = ORIENTED_EDGE ( 'NONE', *, *, #4830, .F. ) ;
#16679 = ORIENTED_EDGE ( 'NONE', *, *, #12729, .F. ) ;
#16680 = DIRECTION ( 'NONE',  ( 0.000000000000000000, 0.000000000000000000, -1.000000000000000000 ) ) ;
#16681 = EDGE_LOOP ( 'NONE', ( #17540, #12902 ) ) ;
#16682 = CIRCLE ( 'NONE', #8114, 0.2952755905511810774 ) ;
#16683 = CARTESIAN_POINT ( 'NONE',  ( -0.3215969074633125979, 0.3838795254899315390, 0.09684874903502814492 ) ) ;
#16684 = LINE ( 'NONE', #21056, #27458 ) ;
#16685 = B_SPLINE_CURVE_WITH_KNOTS ( 'NONE', 3,
 ( #6382, #8500, #23629, #4265, #24664, #5176, #11680, #24394, #3189, #22563 ),
 .UNSPECIFIED., .F., .F.,
 ( 4, 2, 2, 2, 4 ),
 ( 0.000000000000000000, 0.2499999999999997224, 0.4999999999999994449, 0.7499999999999996669, 1.000000000000000000 ),
 .UNSPECIFIED. ) ;
#16687 = CARTESIAN_POINT ( 'NONE',  ( -0.5476281405333199848, 0.07214854559197045325, 0.9202755905511811330 ) ) ;
#16686 = AXIS2_PLACEMENT_3D ( 'NONE', #5052, #26255, #4777 ) ;
#16688 = ORIENTED_EDGE ( 'NONE', *, *, #13139, .T. ) ;
#16689 = CARTESIAN_POINT ( 'NONE',  ( 0.3680051700917441604, 0.000000000000000000, 0.000000000000000000 ) ) ;
#16690 = VERTEX_POINT ( 'NONE', #16096 ) ;
#16691 = CARTESIAN_POINT ( 'NONE',  ( -7.608238775805210269E-17, -0.6212598425196850238, 0.2574803149606298969 ) ) ;
#16692 = CARTESIAN_POINT ( 'NONE',  ( -0.0005980912172688545225, 0.4999996422873391189, 0.1259302777261166184 ) ) ;
#16693 = CARTESIAN_POINT ( 'NONE',  ( -0.2274877609461333494, -0.4708572476091899550, 0.3331434174514416036 ) ) ;
#16694 = EDGE_CURVE ( 'NONE', #24921, #7271, #11426, .T. ) ;
#16695 = LINE ( 'NONE', #25015, #2385 ) ;
#16696 = ORIENTED_EDGE ( 'NONE', *, *, #9036, .T. ) ;
#16697 = CARTESIAN_POINT ( 'NONE',  ( -0.1707210962531915677, -0.4707890492249701131, 0.09685039370078740717 ) ) ;
#16698 = ORIENTED_EDGE ( 'NONE', *, *, #27300, .F. ) ;
#16699 = CARTESIAN_POINT ( 'NONE',  ( 0.04380447413658629385, 0.3324885138898144854, 1.953740157480315043 ) ) ;
#16700 = CARTESIAN_POINT ( 'NONE',  ( 0.03349795313024073878, -0.5118110236220473341, -1.550196850393700920 ) ) ;
#16701 = CIRCLE ( 'NONE', #50, 1.131889763779527547 ) ;
#16702 = FACE_OUTER_BOUND ( 'NONE', #9489, .T. ) ;
#16703 = CARTESIAN_POINT ( 'NONE',  ( -0.5335524835331961757, -0.1429116519061072454, 0.9399606299212598381 ) ) ;
#16704 = ORIENTED_EDGE ( 'NONE', *, *, #19746, .T. ) ;
#16705 = CARTESIAN_POINT ( 'NONE',  ( 0.2847264097284254447, 0.000000000000000000, -3.149606299191693548 ) ) ;
#16706 = CIRCLE ( 'NONE', #18955, 0.3135473077061334268 ) ;
#16707 = VERTEX_POINT ( 'NONE', #13541 ) ;
#16708 = EDGE_CURVE ( 'NONE', #24827, #11368, #7209, .T. ) ;
#16709 = CARTESIAN_POINT ( 'NONE',  ( -0.1649135259639237794, 0.4856708409191340947, -1.550196850393700920 ) ) ;
#16710 = ORIENTED_EDGE ( 'NONE', *, *, #14034, .F. ) ;
#16711 = DIRECTION ( 'NONE',  ( 1.000000000000000000, 0.000000000000000000, 0.000000000000000000 ) ) ;
#16712 = CARTESIAN_POINT ( 'NONE',  ( 0.3339160553493882300, 1.241955529277656956, -0.7081600496628898123 ) ) ;
#16713 = CARTESIAN_POINT ( 'NONE',  ( -0.1220886091248651606, -0.3369140789097872513, 0.1805249803346592186 ) ) ;
#16714 = DIRECTION ( 'NONE',  ( -1.000000000000000000, -1.224646799147356165E-16, 0.000000000000000000 ) ) ;
#16715 = ORIENTED_EDGE ( 'NONE', *, *, #27081, .T. ) ;
#16716 = CARTESIAN_POINT ( 'NONE',  ( -0.5677494271516411173, -0.6030950601078316486, 0.9382339938615534836 ) ) ;
#16717 = ORIENTED_EDGE ( 'NONE', *, *, #3847, .T. ) ;
#16718 = CARTESIAN_POINT ( 'NONE',  ( -2.685748425196850164E-17, 0.000000000000000000, -3.666338582670846780 ) ) ;
#16719 = EDGE_CURVE ( 'NONE', #13737, #11023, #2664, .T. ) ;
#16720 = CARTESIAN_POINT ( 'NONE',  ( 0.000000000000000000, 0.000000000000000000, 0.1992125984251968684 ) ) ;
#16721 = LINE ( 'NONE', #1884, #24425 ) ;
#16722 = DIRECTION ( 'NONE',  ( 1.224646799147353207E-16, 1.000000000000000000, -0.000000000000000000 ) ) ;
#16723 = ORIENTED_EDGE ( 'NONE', *, *, #10194, .T. ) ;
#16724 = AXIS2_PLACEMENT_3D ( 'NONE', #20288, #16198, #22262 ) ;
#16725 = ORIENTED_EDGE ( 'NONE', *, *, #21514, .T. ) ;
#16726 = CARTESIAN_POINT ( 'NONE',  ( -0.02345921195929173697, -0.3574989824755908652, -3.115157480314960647 ) ) ;
#16727 = CARTESIAN_POINT ( 'NONE',  ( 0.2268989272875726881, 0.3929158813954875540, -1.934055118110236338 ) ) ;
#16728 = CARTESIAN_POINT ( 'NONE',  ( -0.4555658499976060760, 0.06001958459474820984, -1.928289503579160513 ) ) ;
#16729 = ADVANCED_FACE ( 'NONE', ( #9431, #22444 ), #13830, .T. ) ;
#16730 = AXIS2_PLACEMENT_3D ( 'NONE', #7864, #1234, #3463 ) ;
#16731 = ORIENTED_EDGE ( 'NONE', *, *, #20438, .F. ) ;
#16732 = EDGE_LOOP ( 'NONE', ( #11823, #6047, #21027, #19544 ) ) ;
#16733 = ORIENTED_EDGE ( 'NONE', *, *, #6812, .T. ) ;
#16734 = CARTESIAN_POINT ( 'NONE',  ( -0.5439522672647024715, -0.3503951963723378471, 0.02327463819225972577 ) ) ;
#16735 = CARTESIAN_POINT ( 'NONE',  ( 3.616083068348477634E-17, 0.07874015748662489822, 0.2952755905511805778 ) ) ;
#16736 = CARTESIAN_POINT ( 'NONE',  ( -0.5144970376935739109, -0.1378076643338908835, 1.747047244094488194 ) ) ;
#16737 = EDGE_CURVE ( 'NONE', #18698, #15474, #31, .T. ) ;
#16738 = VERTEX_POINT ( 'NONE', #26527 ) ;
#16739 = LENGTH_MEASURE_WITH_UNIT ( LENGTH_MEASURE( 0.02539999999999999897 ), #27202 ) ;
#16740 = ORIENTED_EDGE ( 'NONE', *, *, #23246, .T. ) ;
#16741 = ADVANCED_FACE ( 'NONE', ( #26264, #1496 ), #7060, .T. ) ;
#16742 = CARTESIAN_POINT ( 'NONE',  ( 0.1522836969815822838, -0.2938892803218252081, 0.3971963147669425598 ) ) ;
#16743 = ADVANCED_FACE ( 'NONE', ( #3071, #10107 ), #22984, .T. ) ;
#16744 = FACE_BOUND ( 'NONE', #6163, .T. ) ;
#16745 = CARTESIAN_POINT ( 'NONE',  ( -0.4446020952038907681, 0.000000000000000000, -1.934055118110236338 ) ) ;
#16746 = EDGE_CURVE ( 'NONE', #24053, #26265, #10372, .T. ) ;
#16747 = CARTESIAN_POINT ( 'NONE',  ( 0.3074993854542625304, -0.1775730735577552566, 1.953740157480315043 ) ) ;
#16748 = ORIENTED_EDGE ( 'NONE', *, *, #9458, .T. ) ;
#16749 = ORIENTED_EDGE ( 'NONE', *, *, #5823, .F. ) ;
#16750 = FACE_OUTER_BOUND ( 'NONE', #13290, .T. ) ;
#16752 = CARTESIAN_POINT ( 'NONE',  ( -0.5335524835331961757, -0.1429116519061072454, 0.9399606299212598381 ) ) ;
#16751 = CARTESIAN_POINT ( 'NONE',  ( -0.1918813796216842782, -0.5271897577243779276, 0.2775610236220472093 ) ) ;
#16753 = EDGE_CURVE ( 'NONE', #22409, #25416, #26168, .T. ) ;
#16754 = ORIENTED_EDGE ( 'NONE', *, *, #21609, .T. ) ;
#16755 = ORIENTED_EDGE ( 'NONE', *, *, #17223, .T. ) ;
#16756 = VERTEX_POINT ( 'NONE', #19911 ) ;
#16757 = FACE_OUTER_BOUND ( 'NONE', #6114, .T. ) ;
#16758 = DIRECTION ( 'NONE',  ( 1.000000000000000000, 0.000000000000000000, 0.000000000000000000 ) ) ;
#16759 = CIRCLE ( 'NONE', #20823, 0.4941010236220472751 ) ;
#16760 = CARTESIAN_POINT ( 'NONE',  ( 0.3102476824511484210, 0.1791601451668926315, -3.115157480314960647 ) ) ;
#16761 = DIRECTION ( 'NONE',  ( 0.000000000000000000, 0.000000000000000000, 1.000000000000000000 ) ) ;
#16762 = DIRECTION ( 'NONE',  ( -0.2036417511401761582, -0.4895227362422917006, -0.8478782506317886769 ) ) ;
#16763 = CARTESIAN_POINT ( 'NONE',  ( 0.1181102362204724532, 1.446433227339393765E-17, 0.000000000000000000 ) ) ;
#16764 = AXIS2_PLACEMENT_3D ( 'NONE', #15503, #10833, #17195 ) ;
#16765 = CARTESIAN_POINT ( 'NONE',  ( -0.7283464566929135353, 8.919671568592928630E-17, 0.01181102362204724393 ) ) ;
#16766 = VECTOR ( 'NONE', #3015, 39.37007874015748854 ) ;
#16767 = CARTESIAN_POINT ( 'NONE',  ( 0.3191377210032582123, 0.3812612458985252251, 0.1615162260922596571 ) ) ;
#16768 = LINE ( 'NONE', #18441, #21163 ) ;
#16769 = ORIENTED_EDGE ( 'NONE', *, *, #9735, .T. ) ;
#16770 = CARTESIAN_POINT ( 'NONE',  ( -0.0005710523241063101023, 0.4632828964882294565, 0.1494804572083954508 ) ) ;
#16771 = CARTESIAN_POINT ( 'NONE',  ( 0.2313498293151122209, -0.4793777142568558802, 0.3401591244667909186 ) ) ;
#16772 = DIRECTION ( 'NONE',  ( 0.000000000000000000, 1.000000000000000000, 0.000000000000000000 ) ) ;
#16773 = EDGE_CURVE ( 'NONE', #22917, #12919, #22089, .T. ) ;
#16774 = DIRECTION ( 'NONE',  ( 0.000000000000000000, 0.000000000000000000, -1.000000000000000000 ) ) ;
#16775 = CARTESIAN_POINT ( 'NONE',  ( 0.1712563538833069832, -0.5043504886477723215, 1.747047244094488194 ) ) ;
#16776 = APPLICATION_PROTOCOL_DEFINITION ( 'draft international standard', 'automotive_design', 1998, #6031 ) ;
#16777 = CARTESIAN_POINT ( 'NONE',  ( -0.05118110236220472370, -0.8267716535433071723, 1.012503259137575512E-16 ) ) ;
#16778 = CARTESIAN_POINT ( 'NONE',  ( 0.4441657790108421988, 0.2564944395515498798, 1.747047244094488194 ) ) ;
#16779 = ORIENTED_EDGE ( 'NONE', *, *, #2760, .T. ) ;
#16780 = AXIS2_PLACEMENT_3D ( 'NONE', #10490, #27607, #25483 ) ;
#16781 = ORIENTED_EDGE ( 'NONE', *, *, #723, .F. ) ;
#16782 = CARTESIAN_POINT ( 'NONE',  ( 0.04679574315772144777, 0.3551931031211610912, -3.115157480314960647 ) ) ;
#16783 = VERTEX_POINT ( 'NONE', #984 ) ;
#16784 = CARTESIAN_POINT ( 'NONE',  ( -0.4078284417495566250, 0.4849914877874417218, 0.2481708550933849622 ) ) ;
#16785 = DIRECTION ( 'NONE',  ( -1.000000000000000000, 0.000000000000000000, 0.000000000000000000 ) ) ;
#16786 = B_SPLINE_CURVE_WITH_KNOTS ( 'NONE', 3,
 ( #7760, #11844, #14112, #20466, #7617, #16236 ),
 .UNSPECIFIED., .F., .F.,
 ( 4, 2, 4 ),
 ( 0.3000437156586439613, 0.3015484798814569989, 0.3030532441042709801 ),
 .UNSPECIFIED. ) ;
#16787 = ADVANCED_FACE ( 'NONE', ( #9570 ), #10824, .F. ) ;
#16788 = CARTESIAN_POINT ( 'NONE',  ( -0.08676778863011327947, 0.3239425792934402248, 1.973425196850393970 ) ) ;
#16789 = ORIENTED_EDGE ( 'NONE', *, *, #27081, .F. ) ;
#16790 = ORIENTED_EDGE ( 'NONE', *, *, #25771, .T. ) ;
#16791 = AXIS2_PLACEMENT_3D ( 'NONE', #12637, #21812, #11076 ) ;
#16792 = CARTESIAN_POINT ( 'NONE',  ( 0.3001918266902036669, -0.3912931228432058872, -1.550196850393700920 ) ) ;
#16793 = CARTESIAN_POINT ( 'NONE',  ( -0.5383572925355968319, -0.3100567972183898013, 0.09685039370078740717 ) ) ;
#16794 = ORIENTED_EDGE ( 'NONE', *, *, #6993, .F. ) ;
#16795 = VERTEX_POINT ( 'NONE', #7471 ) ;
#16796 = B_SPLINE_CURVE_WITH_KNOTS ( 'NONE', 3,
 ( #659, #15108, #10987, #23720, #8857, #4354 ),
 .UNSPECIFIED., .F., .F.,
 ( 4, 2, 4 ),
 ( 0.3108507187342950395, 0.3125269569790670166, 0.3142031952238389936 ),
 .UNSPECIFIED. ) ;
#16797 = ITEM_DEFINED_TRANSFORMATION ( 'NONE', 'NONE', #24197,  #11588 ) ;
#16798 = CARTESIAN_POINT ( 'NONE',  ( 0.6202606299212598540, -0.08876456692913387014, 0.000000000000000000 ) ) ;
#16799 = CARTESIAN_POINT ( 'NONE',  ( -0.2425693455392315123, 0.2888145544500153594, 0.1992150590373740204 ) ) ;
#16800 = CARTESIAN_POINT ( 'NONE',  ( 0.000000000000000000, 0.000000000000000000, -0.3779527559055118058 ) ) ;
#16801 = CARTESIAN_POINT ( 'NONE',  ( 0.4714076450718495126, 0.08371568475172405654, 0.08349695147687043184 ) ) ;
#16802 = ORIENTED_EDGE ( 'NONE', *, *, #22850, .F. ) ;
#16803 = B_SPLINE_SURFACE_WITH_KNOTS ( 'NONE', 3, 3, ( 
 ( #9977, #16480, #5610, #20857 ),
 ( #24659, #27221, #5758, #1506 ),
 ( #12100, #22558, #955, #20719 ),
 ( #18730, #1365, #8015, #16620 ) ),
 .UNSPECIFIED., .F., .F., .F.,
 ( 4, 4 ),
 ( 4, 4 ),
 ( -0.1875000000000000000, 0.5625000000000000000 ),
 ( -0.2617993877991500185, 0.2617993877991500185 ),
 .UNSPECIFIED. ) ;
#16804 = AXIS2_PLACEMENT_3D ( 'NONE', #12304, #20929, #3834 ) ;
#16805 = TOROIDAL_SURFACE ( 'NONE', #4602, 0.5610236220472440971, 0.1003937007874015908 ) ;
#16806 = ORIENTED_EDGE ( 'NONE', *, *, #1685, .F. ) ;
#16807 = CARTESIAN_POINT ( 'NONE',  ( -0.5871411068728082938, -0.4592309206872642879, 0.9950886776261244071 ) ) ;
#16808 = CARTESIAN_POINT ( 'NONE',  ( 0.1516263115863346334, -0.4909405214979283838, -0.05579628926458622684 ) ) ;
#16809 = DIRECTION ( 'NONE',  ( 1.000000000000000000, 0.000000000000000000, 0.000000000000000000 ) ) ;
#16810 = DIRECTION ( 'NONE',  ( 0.000000000000000000, 1.000000000000000000, 0.000000000000000000 ) ) ;
#16811 = CARTESIAN_POINT ( 'NONE',  ( -0.05981201256803149457, 1.563633646945708833, 2.145669291338582862 ) ) ;
#16812 = AXIS2_PLACEMENT_3D ( 'NONE', #14861, #12435, #25430 ) ;
#16813 = CARTESIAN_POINT ( 'NONE',  ( -0.6023373761219545930, -0.1921201442084726485, 0.2218210095010204053 ) ) ;
#16814 = DIRECTION ( 'NONE',  ( 0.000000000000000000, -1.000000000000000000, 0.000000000000000000 ) ) ;
#16815 = CARTESIAN_POINT ( 'NONE',  ( -0.09842519685039370636, -0.07874015748031495954, -0.04546065111729338803 ) ) ;
#16816 = CARTESIAN_POINT ( 'NONE',  ( 0.6397637795275591399, 9.642888182262624280E-17, 0.7874015748031496509 ) ) ;
#16817 = PLANE ( 'NONE',  #13958 ) ;
#16818 = EDGE_CURVE ( 'NONE', #19876, #27384, #8567, .T. ) ;
#16819 = PLANE ( 'NONE',  #15888 ) ;
#16820 = ORIENTED_EDGE ( 'NONE', *, *, #14012, .F. ) ;
#16821 = DIRECTION ( 'NONE',  ( -1.000000000000000000, 0.000000000000000000, 0.000000000000000000 ) ) ;
#16822 = ORIENTED_EDGE ( 'NONE', *, *, #27734, .F. ) ;
#16823 = CARTESIAN_POINT ( 'NONE',  ( 0.2992781133268291316, -0.6197069291944922176, 0.1322834645669291320 ) ) ;
#16824 = EDGE_CURVE ( 'NONE', #15542, #27306, #12230, .T. ) ;
#16825 = ORIENTED_EDGE ( 'NONE', *, *, #17689, .F. ) ;
#16826 = VECTOR ( 'NONE', #20964, 39.37007874015748143 ) ;
#16827 = ORIENTED_EDGE ( 'NONE', *, *, #11608, .T. ) ;
#16828 = CARTESIAN_POINT ( 'NONE',  ( -0.5858067486093416765, 1.092930385925676040, -0.09774754414358965970 ) ) ;
#16829 = DIRECTION ( 'NONE',  ( -0.000000000000000000, -0.000000000000000000, 1.000000000000000000 ) ) ;
#16830 = DIRECTION ( 'NONE',  ( 0.000000000000000000, 0.000000000000000000, -1.000000000000000000 ) ) ;
#16831 = ORIENTED_EDGE ( 'NONE', *, *, #24508, .T. ) ;
#16832 = ADVANCED_FACE ( 'NONE', ( #562 ), #24553, .F. ) ;
#16833 = CARTESIAN_POINT ( 'NONE',  ( 0.6299212598425196763, -0.07910393700787400617, 0.000000000000000000 ) ) ;
#16834 = ORIENTED_EDGE ( 'NONE', *, *, #11882, .F. ) ;
#16835 = AXIS2_PLACEMENT_3D ( 'NONE', #17459, #15758, #21840 ) ;
#16836 = CARTESIAN_POINT ( 'NONE',  ( 0.2952755905511810774, 0.000000000000000000, 0.01181102362204724393 ) ) ;
#16837 = CARTESIAN_POINT ( 'NONE',  ( -0.2089723435111595362, -0.4324731448915372645, 0.2529987172187860844 ) ) ;
#16838 = ADVANCED_FACE ( 'NONE', ( #18719 ), #21661, .T. ) ;
#16839 = DIRECTION ( 'NONE',  ( -1.000000000000000000, 0.000000000000000000, -0.000000000000000000 ) ) ;
#16840 = EDGE_LOOP ( 'NONE', ( #16276, #19733, #26817, #2117 ) ) ;
#16841 = CARTESIAN_POINT ( 'NONE',  ( -9.069736220472442904E-16, -0.8267716535433071723, 0.000000000000000000 ) ) ;
#16842 = EDGE_LOOP ( 'NONE', ( #24381, #1281 ) ) ;
#16843 = CARTESIAN_POINT ( 'NONE',  ( 0.3324885138898234782, -0.04380447413659139394, 1.973425196850393970 ) ) ;
#16844 = AXIS2_PLACEMENT_3D ( 'NONE', #18927, #14733, #23338 ) ;
#16845 = CARTESIAN_POINT ( 'NONE',  ( 0.000000000000000000, 0.000000000000000000, 0.1377952755905511861 ) ) ;
#16846 = AXIS2_PLACEMENT_3D ( 'NONE', #21215, #1855, #19080 ) ;
#16847 = CARTESIAN_POINT ( 'NONE',  ( -0.07214854559199535000, -0.5476281405333250918, 0.9399606299212598381 ) ) ;
#16848 = FACE_OUTER_BOUND ( 'NONE', #21935, .T. ) ;
#16849 = CARTESIAN_POINT ( 'NONE',  ( 0.000000000000000000, 0.000000000000000000, 0.2637795275590551491 ) ) ;
#16850 = DIRECTION ( 'NONE',  ( 0.000000000000000000, 0.000000000000000000, -1.000000000000000000 ) ) ;
#16851 = ORIENTED_EDGE ( 'NONE', *, *, #871, .F. ) ;
#16852 = CARTESIAN_POINT ( 'NONE',  ( 0.000000000000000000, 0.000000000000000000, -3.149606299191693548 ) ) ;
#16853 = DIRECTION ( 'NONE',  ( -1.147443000000000016E-15, -1.000000000000000000, -0.000000000000000000 ) ) ;
#16854 = TOROIDAL_SURFACE ( 'NONE', #8740, 0.7165354330708662012, 0.01181102362204724393 ) ;
#16855 = DIRECTION ( 'NONE',  ( 1.000000000000000000, 0.000000000000000000, 0.000000000000000000 ) ) ;
#16856 = ADVANCED_FACE ( 'NONE', ( #18855, #27502 ), #23268, .T. ) ;
#16857 = ORIENTED_EDGE ( 'NONE', *, *, #27605, .T. ) ;
#16858 = EDGE_CURVE ( 'NONE', #16039, #16425, #21131, .T. ) ;
#16859 = CARTESIAN_POINT ( 'NONE',  ( 0.4069448477569526101, -0.3121994997578271813, -1.550196850393700920 ) ) ;
#16860 = CARTESIAN_POINT ( 'NONE',  ( -0.5708661417322835607, -0.03747632742162953362, 0.9399606299212600602 ) ) ;
#16861 = CARTESIAN_POINT ( 'NONE',  ( 0.6106000000000000316, -1.355930314960630041E-19, 0.000000000000000000 ) ) ;
#16862 = DIRECTION ( 'NONE',  ( -1.000000000000000000, 0.000000000000000000, 0.000000000000000000 ) ) ;
#16863 = CARTESIAN_POINT ( 'NONE',  ( 0.06947618719649770180, -0.5280904602948609528, 1.747047244094488416 ) ) ;
#16864 = CLOSED_SHELL ( 'NONE', ( #20339, #22513, #26064, #483, #14245, #12915, #11184, #26848, #27434, #7953, #6259, #20317, #10756, #24663, #8773, #7248, #1955, #7797, #3106, #8649, #10942, #7138, #15367, #10526, #18808, #7705, #11802, #1667, #12951 ) ) ;
#16865 = CARTESIAN_POINT ( 'NONE',  ( -7.279147705782180972E-18, 0.5322834645669292097, 0.1322810039474933141 ) ) ;
#16866 = CARTESIAN_POINT ( 'NONE',  ( 0.000000000000000000, 0.000000000000000000, 0.4488188976377953110 ) ) ;
#16867 = ORIENTED_EDGE ( 'NONE', *, *, #19489, .T. ) ;
#16868 = VECTOR ( 'NONE', #17992, 39.37007874015748854 ) ;
#16869 = DIRECTION ( 'NONE',  ( -0.9848077530122080203, 0.1736481776669311083, 0.000000000000000000 ) ) ;
#16870 = CIRCLE ( 'NONE', #7370, 0.5570866141732283561 ) ;
#16871 = CARTESIAN_POINT ( 'NONE',  ( -0.5660396215081976434, -0.5184600247624503444, -0.9894322414029975699 ) ) ;
#16872 = CYLINDRICAL_SURFACE ( 'NONE', #1816, 0.6212598425196850238 ) ;
#16873 = CYLINDRICAL_SURFACE ( 'NONE', #21742, 0.7874015748031496509 ) ;
#16874 = CARTESIAN_POINT ( 'NONE',  ( -0.6265112766918068399, -0.4592307444201776945, -0.9950886577925649457 ) ) ;
#16875 = ORIENTED_EDGE ( 'NONE', *, *, #15743, .F. ) ;
#16876 = FILL_AREA_STYLE_COLOUR ( '', #16618 ) ;
#16877 = AXIS2_PLACEMENT_3D ( 'NONE', #20445, #3331, #7444 ) ;
#16878 = CARTESIAN_POINT ( 'NONE',  ( -0.3012109481301850633, 0.3598698725862389813, 0.1992125984251968684 ) ) ;
#16879 = AXIS2_PLACEMENT_3D ( 'NONE', #9742, #715, #9305 ) ;
#16880 = ORIENTED_EDGE ( 'NONE', *, *, #15441, .F. ) ;
#16881 = FILL_AREA_STYLE_COLOUR ( '', #25162 ) ;
#16882 = CARTESIAN_POINT ( 'NONE',  ( -0.4143458349595040002, -0.2398979215380011853, 0.08349695147757887903 ) ) ;
#16883 = CARTESIAN_POINT ( 'NONE',  ( 0.4423390553432409722, -0.2180862235769587265, -1.569881889763779625 ) ) ;
#16884 = EDGE_CURVE ( 'NONE', #3542, #4805, #8285, .T. ) ;
#16885 = CARTESIAN_POINT ( 'NONE',  ( -0.4351030398461734339, 0.1477428134820354677, -1.928289503579158959 ) ) ;
#16886 = ORIENTED_EDGE ( 'NONE', *, *, #4386, .T. ) ;
#16887 = CARTESIAN_POINT ( 'NONE',  ( -0.6068752646683485130, -0.1116593662105169332, -0.2438664148410240040 ) ) ;
#16888 = DIRECTION ( 'NONE',  ( -0.9396926207859082059, -0.3420201433256690460, 0.000000000000000000 ) ) ;
#16889 = EDGE_LOOP ( 'NONE', ( #6746, #7461, #1603, #27127 ) ) ;
#16890 = CARTESIAN_POINT ( 'NONE',  ( -0.3056525133683296036, 0.3651631491442455246, 0.1212655228852408396 ) ) ;
#16891 = ORIENTED_EDGE ( 'NONE', *, *, #10960, .T. ) ;
#16892 = AXIS2_PLACEMENT_3D ( 'NONE', #26017, #10903, #2681 ) ;
#16893 = CARTESIAN_POINT ( 'NONE',  ( -0.4055118110236220486, 0.9448818897637796255, -9.561468503937007847E-18 ) ) ;
#16894 = AXIS2_PLACEMENT_3D ( 'NONE', #27741, #1736, #23223 ) ;
#16895 = CARTESIAN_POINT ( 'NONE',  ( 0.4067073728345788064, -0.2341441294389338956, 0.1992125984251968684 ) ) ;
#16896 = DIRECTION ( 'NONE',  ( 0.000000000000000000, -1.000000000000000000, 0.000000000000000000 ) ) ;
#16897 = ORIENTED_EDGE ( 'NONE', *, *, #13797, .F. ) ;
#16898 = CARTESIAN_POINT ( 'NONE',  ( 0.02319089060378217229, -0.3543307086614173596, 1.953740157480315043 ) ) ;
#16899 = ORIENTED_EDGE ( 'NONE', *, *, #16234, .F. ) ;
#16900 = CARTESIAN_POINT ( 'NONE',  ( -0.5857032253883902584, -0.1585179380598580323, -0.2517153213116811727 ) ) ;
#16902 = CARTESIAN_POINT ( 'NONE',  ( -0.5526079293736928522, -0.1480156394741928838, 0.9399606299212598381 ) ) ;
#16901 = CYLINDRICAL_SURFACE ( 'NONE', #2704, 0.4986013261500205074 ) ;
#16903 = ORIENTED_EDGE ( 'NONE', *, *, #27839, .T. ) ;
#16904 = FACE_OUTER_BOUND ( 'NONE', #13110, .T. ) ;
#16905 = DIRECTION ( 'NONE',  ( 0.000000000000000000, 1.000000000000000000, 0.000000000000000000 ) ) ;
#16906 = CARTESIAN_POINT ( 'NONE',  ( -0.2842490391651530390, -0.2180698645301770988, -3.115157480314960647 ) ) ;
#16907 = LINE ( 'NONE', #21552, #21157 ) ;
#16908 = CARTESIAN_POINT ( 'NONE',  ( 0.0005939837304750000086, 0.5007870493127504208, 0.2574803149606298969 ) ) ;
#16909 = LINE ( 'NONE', #21426, #22095 ) ;
#16910 = EDGE_CURVE ( 'NONE', #3844, #24509, #7830, .T. ) ;
#16911 = EDGE_CURVE ( 'NONE', #10134, #20290, #25267, .T. ) ;
#16912 = DIRECTION ( 'NONE',  ( 1.000000000000000000, 0.000000000000000000, 0.000000000000000000 ) ) ;
#16913 = CIRCLE ( 'NONE', #4285, 1.092519685039370136 ) ;
#16914 = CARTESIAN_POINT ( 'NONE',  ( 0.6175000359513720394, 0.5735261876549937465, -0.4659829881745126134 ) ) ;
#16915 = PRODUCT_RELATED_PRODUCT_CATEGORY ( 'part', '', ( #16553 ) ) ;
#16916 = AXIS2_PLACEMENT_3D ( 'NONE', #26858, #17456, #19717 ) ;
#16917 = DIRECTION ( 'NONE',  ( 1.000000000000000000, 0.000000000000000000, 0.000000000000000000 ) ) ;
#16918 = EDGE_CURVE ( 'NONE', #730, #27022, #14910, .T. ) ;
#16919 = ORIENTED_EDGE ( 'NONE', *, *, #14676, .T. ) ;
#16920 = CARTESIAN_POINT ( 'NONE',  ( -0.01968503937007873988, 0.6246466694403326469, 7.649715443281581808E-17 ) ) ;
#16921 = CARTESIAN_POINT ( 'NONE',  ( 0.000000000000000000, 0.000000000000000000, 0.09685039370078740717 ) ) ;
#16922 = VERTEX_POINT ( 'NONE', #24765 ) ;
#16923 = ORIENTED_EDGE ( 'NONE', *, *, #7983, .F. ) ;
#16924 = ADVANCED_FACE ( 'NONE', ( #11498 ), #9360, .T. ) ;
#16925 = VERTEX_POINT ( 'NONE', #17965 ) ;
#16926 = DIRECTION ( 'NONE',  ( 0.2036417511401770464, 0.4895227362422922002, 0.8478782506317882328 ) ) ;
#16927 = CARTESIAN_POINT ( 'NONE',  ( 0.000000000000000000, 0.000000000000000000, 0.1377952755905511584 ) ) ;
#16928 = ORIENTED_EDGE ( 'NONE', *, *, #20172, .F. ) ;
#16929 = VERTEX_POINT ( 'NONE', #5568 ) ;
#16930 = CARTESIAN_POINT ( 'NONE',  ( 0.2693339498142349187, -0.2362439534887297299, -3.115157480314960647 ) ) ;
#16931 = VERTEX_POINT ( 'NONE', #5428 ) ;
#16932 = DIRECTION ( 'NONE',  ( 1.000000000000000000, 0.000000000000000000, -0.000000000000000000 ) ) ;
#16933 = ORIENTED_EDGE ( 'NONE', *, *, #723, .T. ) ;
#16934 = CARTESIAN_POINT ( 'NONE',  ( 0.000000000000000000, 0.000000000000000000, 0.7844728274238290666 ) ) ;
#16935 = CARTESIAN_POINT ( 'NONE',  ( -0.3239425792934405024, 0.08676778863011171128, 1.973425196850393970 ) ) ;
#16936 = ORIENTED_EDGE ( 'NONE', *, *, #14157, .T. ) ;
#16937 = ORIENTED_EDGE ( 'NONE', *, *, #14171, .T. ) ;
#16938 = CIRCLE ( 'NONE', #11055, 0.4606299212598425341 ) ;
#16939 = CARTESIAN_POINT ( 'NONE',  ( 0.4669911931914963454, -0.1585706980422251222, -1.550196850393700920 ) ) ;
#16940 = AXIS2_PLACEMENT_3D ( 'NONE', #15007, #23624, #13001 ) ;
#16941 = EDGE_LOOP ( 'NONE', ( #27145, #25503, #20106, #16592 ) ) ;
#16942 = EDGE_LOOP ( 'NONE', ( #27654, #3264 ) ) ;
#16943 = ITEM_DEFINED_TRANSFORMATION ( 'NONE', 'NONE', #25161,  #11588 ) ;
#16944 = DIRECTION ( 'NONE',  ( 1.000000000000000000, 0.000000000000000000, 0.000000000000000000 ) ) ;
#16945 = DIRECTION ( 'NONE',  ( 1.000000000000000000, 0.000000000000000000, 0.000000000000000000 ) ) ;
#16946 = DIRECTION ( 'NONE',  ( 0.000000000000000000, -1.000000000000000000, 0.000000000000000000 ) ) ;
#16947 = CARTESIAN_POINT ( 'NONE',  ( 0.03532354024591839031, -0.6299212598425196763, 0.000000000000000000 ) ) ;
#16948 = EDGE_CURVE ( 'NONE', #12564, #23913, #1331, .T. ) ;
#16949 = DIRECTION ( 'NONE',  ( 0.000000000000000000, 0.000000000000000000, 1.000000000000000000 ) ) ;
#16950 = CARTESIAN_POINT ( 'NONE',  ( 0.1659602483926377881, 2.925196850393700920, 0.7677165354330708347 ) ) ;
#16951 = VECTOR ( 'NONE', #755, 39.37007874015748143 ) ;
#16952 = CARTESIAN_POINT ( 'NONE',  ( -0.5356467622208501700, -0.4294193594449044471, 0.1625794819182737050 ) ) ;
#16953 = CARTESIAN_POINT ( 'NONE',  ( -0.1200170377978882624, 0.4465874321618641951, -1.928289503579156960 ) ) ;
#16954 = EDGE_CURVE ( 'NONE', #27811, #12956, #16701, .T. ) ;
#16955 = CARTESIAN_POINT ( 'NONE',  ( 0.3346456692913385988, 4.098227477461614641E-17, 2.504921259842519898 ) ) ;
#16956 = CARTESIAN_POINT ( 'NONE',  ( -0.6205616028481958368, -0.4724399524669597450, 0.9954595399567032210 ) ) ;
#16957 = CARTESIAN_POINT ( 'NONE',  ( 0.02061007003135907623, 0.1968503937007873850, -3.195947033497543721 ) ) ;
#16958 = DIRECTION ( 'NONE',  ( 3.169619147893061878E-17, -0.9659258263664941557, 0.2588190448135637145 ) ) ;
#16959 = EDGE_LOOP ( 'NONE', ( #7555, #17987, #17858, #27674 ) ) ;
#16960 = DIRECTION ( 'NONE',  ( 1.000000000000000000, 0.000000000000000000, 0.000000000000000000 ) ) ;
#16961 = AXIS2_PLACEMENT_3D ( 'NONE', #16893, #18995, #14928 ) ;
#16962 = ADVANCED_FACE ( 'NONE', ( #18539 ), #12626, .T. ) ;
#16963 = ORIENTED_EDGE ( 'NONE', *, *, #24423, .F. ) ;
#16964 = CARTESIAN_POINT ( 'NONE',  ( 0.09590060490395689585, 0.1136516277932340530, -0.1968503937007874127 ) ) ;
#16965 = FACE_OUTER_BOUND ( 'NONE', #20141, .T. ) ;
#16966 = DIRECTION ( 'NONE',  ( -0.000000000000000000, -0.000000000000000000, -1.000000000000000000 ) ) ;
#16967 = CARTESIAN_POINT ( 'NONE',  ( 0.4783323773986568606, 0.2762247810518930202, 0.9202755905511811330 ) ) ;
#16968 = ORIENTED_EDGE ( 'NONE', *, *, #10642, .T. ) ;
#16969 = CARTESIAN_POINT ( 'NONE',  ( 0.000000000000000000, 0.000000000000000000, 0.01181102362204724393 ) ) ;
#16970 = ORIENTED_EDGE ( 'NONE', *, *, #2729, .T. ) ;
#16971 = CARTESIAN_POINT ( 'NONE',  ( 0.2847264097284254447, 0.000000000000000000, -3.149606299191693548 ) ) ;
#16972 = CIRCLE ( 'NONE', #17403, 0.09143349766193348271 ) ;
#16973 = CARTESIAN_POINT ( 'NONE',  ( -0.4792483803617587634, 0.08390985360245291347, 0.2467937632999436248 ) ) ;
#16974 = DIRECTION ( 'NONE',  ( 0.000000000000000000, 0.000000000000000000, 1.000000000000000000 ) ) ;
#16975 = EDGE_CURVE ( 'NONE', #27484, #3132, #3445, .T. ) ;
#16976 = CIRCLE ( 'NONE', #26903, 0.3294268239956709143 ) ;
#16977 = B_SPLINE_CURVE_WITH_KNOTS ( 'NONE', 2,
 ( #17824, #12805, #2069 ),
 .UNSPECIFIED., .F., .F.,
 ( 3, 3 ),
 ( 0.000000000000000000, 1.000000000000000000 ),
 .UNSPECIFIED. ) ;
#16978 = DIRECTION ( 'NONE',  ( 0.000000000000000000, 0.000000000000000000, 1.000000000000000000 ) ) ;
#16979 = VERTEX_POINT ( 'NONE', #16169 ) ;
#16980 = CARTESIAN_POINT ( 'NONE',  ( 0.3937007874015748254, 0.000000000000000000, 0.4488188976377953110 ) ) ;
#16981 = CARTESIAN_POINT ( 'NONE',  ( -0.09842519685039366473, 0.1968503937007873850, -3.364501312335960836 ) ) ;
#16982 = EDGE_LOOP ( 'NONE', ( #20364, #10586, #7361, #24614 ) ) ;
#16983 = DIRECTION ( 'NONE',  ( 0.000000000000000000, 0.000000000000000000, 1.000000000000000000 ) ) ;
#16984 = EDGE_CURVE ( 'NONE', #16322, #13098, #4518, .T. ) ;
#16985 = DIRECTION ( 'NONE',  ( -1.000000000000000000, 0.000000000000000000, -0.000000000000000000 ) ) ;
#16986 = CARTESIAN_POINT ( 'NONE',  ( 0.2442565704126269388, 0.4954197419817067960, 0.9399606299212598381 ) ) ;
#16987 = DIRECTION ( 'NONE',  ( 0.000000000000000000, 1.000000000000000000, 0.000000000000000000 ) ) ;
#16988 = ORIENTED_EDGE ( 'NONE', *, *, #25408, .F. ) ;
#16989 = CARTESIAN_POINT ( 'NONE',  ( 0.3213059197595201644, 0.1584813376848823729, -3.115157480314960647 ) ) ;
#16990 = ADVANCED_FACE ( 'NONE', ( #1197 ), #16239, .F. ) ;
#16991 = VECTOR ( 'NONE', #22028, 39.37007874015748143 ) ;
#16992 = ADVANCED_FACE ( 'NONE', ( #22656 ), #4057, .F. ) ;
#16993 = ORIENTED_EDGE ( 'NONE', *, *, #14857, .T. ) ;
#16994 = CIRCLE ( 'NONE', #22386, 0.1673228346456692994 ) ;
#16995 = CARTESIAN_POINT ( 'NONE',  ( 0.1649135259639267770, -0.4856708409191258236, -1.550196850393700920 ) ) ;
#16996 = CARTESIAN_POINT ( 'NONE',  ( -0.3986320731132244610, -0.2308081338369635804, 0.1771653543307087630 ) ) ;
#16997 = DIRECTION ( 'NONE',  ( 0.000000000000000000, -1.000000000000000000, 0.000000000000000000 ) ) ;
#16998 = DIRECTION ( 'NONE',  ( 0.000000000000000000, 0.000000000000000000, -1.000000000000000000 ) ) ;
#16999 = DIRECTION ( 'NONE',  ( 0.000000000000000000, -1.000000000000000000, 0.000000000000000000 ) ) ;
#17000 = B_SPLINE_CURVE_WITH_KNOTS ( 'NONE', 3,
 ( #27580, #8222, #19658, #327, #4537, #21636, #13142, #13007, #19785, #19228 ),
 .UNSPECIFIED., .F., .F.,
 ( 4, 2, 2, 2, 4 ),
 ( 0.000000000000000000, 0.2500000000000000000, 0.5000000000000000000, 0.7500000000000000000, 1.000000000000000000 ),
 .UNSPECIFIED. ) ;
#17001 = DIRECTION ( 'NONE',  ( 1.000000000000000000, 0.000000000000000000, 0.000000000000000000 ) ) ;
#17002 = ORIENTED_EDGE ( 'NONE', *, *, #18180, .T. ) ;
#17003 = CARTESIAN_POINT ( 'NONE',  ( 0.6241887519799541595, -0.3029073140874564696, 0.5246508579836981490 ) ) ;
#17004 = CARTESIAN_POINT ( 'NONE',  ( 0.1718374205099799101, -0.4703827404237102550, 0.09685039370078740717 ) ) ;
#17005 = CARTESIAN_POINT ( 'NONE',  ( 0.2249706821157846648, -0.9514344361775100012, -0.1680475531490076835 ) ) ;
#17006 = CARTESIAN_POINT ( 'NONE',  ( 0.6106000000000000316, -1.355930314960630041E-19, 0.000000000000000000 ) ) ;
#17007 = EDGE_LOOP ( 'NONE', ( #4992, #20561 ) ) ;
#17008 = ADVANCED_FACE ( 'NONE', ( #13754, #18098 ), #26744, .T. ) ;
#17009 = CARTESIAN_POINT ( 'NONE',  ( -0.5905511811023621549, 0.9448818897637796255, -1.639108661417322569E-17 ) ) ;
#17010 = DIRECTION ( 'NONE',  ( 0.000000000000000000, 0.000000000000000000, 1.000000000000000000 ) ) ;
#17011 = CARTESIAN_POINT ( 'NONE',  ( -0.002724751885584093553, 0.000000000000000000, 0.1968503937007874127 ) ) ;
#17012 = AXIS2_PLACEMENT_3D ( 'NONE', #17307, #499, #19976 ) ;
#17013 = B_SPLINE_CURVE_WITH_KNOTS ( 'NONE', 3,
 ( #11114, #17862, #15101, #19734, #13365, #26089 ),
 .UNSPECIFIED., .F., .F.,
 ( 4, 1, 1, 4 ),
 ( 0.000000000000000000, 0.4285714285714280480, 0.7142857142857139685, 1.000000000000000000 ),
 .UNSPECIFIED. ) ;
#17014 = VERTEX_POINT ( 'NONE', #22518 ) ;
#17015 = CARTESIAN_POINT ( 'NONE',  ( -0.07874015748031495954, -0.03414999754207796723, -0.4724409448818898127 ) ) ;
#17016 = CARTESIAN_POINT ( 'NONE',  ( 0.1585706980422246781, 0.4669911931914895176, -1.550196850393700920 ) ) ;
#17017 = EDGE_CURVE ( 'NONE', #25537, #18462, #3146, .T. ) ;
#17018 = PRODUCT_DEFINITION_CONTEXT ( 'detailed design', #4568, 'design' ) ;
#17019 = ORIENTED_EDGE ( 'NONE', *, *, #20768, .T. ) ;
#17020 = CARTESIAN_POINT ( 'NONE',  ( 0.3599896729929412120, -0.2761764805255614297, -1.934055118110236338 ) ) ;
#17021 = COLOUR_RGB ( '', 0.72549020, 0.75294118, 0.79215686) ;
#17022 = CARTESIAN_POINT ( 'NONE',  ( -0.3082037322265121504, 0.3663931537949983164, 0.08349695147730891442 ) ) ;
#17023 = EDGE_LOOP ( 'NONE', ( #6554, #21897, #24404, #23016, #10379, #10082, #27278 ) ) ;
#17024 = CARTESIAN_POINT ( 'NONE',  ( -0.6068752646683485130, -0.1762754969233277791, 0.2241499015451751953 ) ) ;
#17025 = CARTESIAN_POINT ( 'NONE',  ( 0.000000000000000000, 0.000000000000000000, 0.09685039370078740717 ) ) ;
#17026 = CARTESIAN_POINT ( 'NONE',  ( -0.2973550541829020344, 0.3552623538055160179, 0.1494804572073591964 ) ) ;
#17027 = EDGE_CURVE ( 'NONE', #25537, #3239, #23477, .T. ) ;
#17028 = EDGE_LOOP ( 'NONE', ( #9889, #8206, #11013, #14186 ) ) ;
#17029 = CARTESIAN_POINT ( 'NONE',  ( -0.6710470464557992676, -0.1526433524317946933, 0.3401591245381555551 ) ) ;
#17030 = AXIS2_PLACEMENT_3D ( 'NONE', #27139, #5379, #14001 ) ;
#17031 = DIRECTION ( 'NONE',  ( 0.000000000000000000, 1.000000000000000000, 0.000000000000000000 ) ) ;
#17032 = B_SPLINE_SURFACE_WITH_KNOTS ( 'NONE', 2, 3, ( 
 ( #25672, #271, #17059, #19166, #23964, #2339, #8, #17332, #17193, #4478, #6600, #2484, #4598, #19726, #8710, #10969, #19594, #21712, #8843, #23569, #396, #19308, #1937, #8974, #2209, #15225, #17466, #23838, #27803, #21298, #13088, #23432, #14956, #26080, #4065, #10545, #8438, #6326, #4202, #138, #12808, #21436, #2077, #10690, #25809, #6458, #15093, #23703, #4339, #12942, #21573, #3016, #11236, #13776, #15767, #1075, #3163, #7414, #13922, #9673, #9522, #18118, #11796, #9109, #11516, #22394 ),
 ( #26480, #19861, #18271, #17984, #22537, #20132, #24369, #20413, #7276, #26913, #20273, #792, #15502, #24100, #11654, #933, #2882, #5297, #26619, #17728, #4735, #26765, #15633, #5011, #9378, #7012, #13357, #15895, #517, #21982, #24498, #2615, #26350, #22251, #16042, #19996, #13630, #5149, #24638, #24236, #4875, #13489, #22116, #7144, #2745, #11377, #649, #9239, #17857, #24785, #18991, #22675, #7560, #16186, #7991, #16458, #12357, #16325, #14063, #12502, #22822, #14215, #1481, #5876, #20559, #25071 ),
 ( #10093, #20976, #18702, #11942, #5450, #16596, #3883, #27060, #14503, #3302, #1620, #27339, #10370, #21117, #3584, #1212, #22965, #25209, #23106, #3735, #10224, #18416, #14352, #7712, #27200, #23251, #18840, #5585, #27481, #7849, #1757, #3440, #8127, #6012, #12077, #16736, #25349, #20696, #14649, #18556, #5735, #12217, #13182, #10798, #6567, #2448, #17429, #25501, #4028, #27764, #6166, #6291, #25776, #15189, #21263, #19556, #21679, #4167, #2307, #12774, #26045, #10507, #21400, #2040, #10653, #19273 ) ),
 .UNSPECIFIED., .F., .T., .F.,
 ( 3, 3 ),
 ( 4, 2, 2, 2, 2, 2, 2, 2, 2, 2, 2, 2, 2, 2, 2, 2, 2, 2, 2, 2, 2, 2, 2, 2, 2, 2, 2, 2, 2, 2, 2, 2, 4 ),
 ( 0.000000000000000000, 1.000000000000000000 ),
 ( 0.000000000000000000, 0.1963495408493620697, 0.3926990816987241395, 0.5890486225480862092, 0.7853981633974482790, 0.9817477042468103487, 1.178097245096172418, 1.374446785945534488, 1.570796326794896558, 1.767145867644258628, 1.963495408493620697, 2.159844949342982545, 2.356194490192344837, 2.552544031041707129, 2.748893571891068976, 2.945243112740430824, 3.141592653589793116, 3.337942194439155408, 3.534291735288517255, 3.730641276137879103, 3.926990816987241395, 4.123340357836603687, 4.319689898685965090, 4.516039439535327382, 4.712388980384689674, 4.908738521234051966, 5.105088062083414258, 5.301437602932775661, 5.497787143782137953, 5.694136684631500245, 5.890486225480861648, 6.086835766330223940, 6.283185307179586232 ),
 .UNSPECIFIED. ) ;
#17033 = CARTESIAN_POINT ( 'NONE',  ( -0.1981752911889803626, -0.1315891372465754772, 0.2362204724409455170 ) ) ;
#17034 = ORIENTED_EDGE ( 'NONE', *, *, #13968, .T. ) ;
#17035 = CARTESIAN_POINT ( 'NONE',  ( -0.02319089060378155473, 0.3543307086614173596, 1.953740157480315043 ) ) ;
#17036 = VERTEX_POINT ( 'NONE', #4012 ) ;
#17037 = CARTESIAN_POINT ( 'NONE',  ( -0.6233626497309882053, -0.07482011975815597293, -0.2396529498863955721 ) ) ;
#17038 = FACE_OUTER_BOUND ( 'NONE', #23186, .T. ) ;
#17039 = CARTESIAN_POINT ( 'NONE',  ( 0.2860899518037616773, -0.4954156765914850546, 0.9399606299212598381 ) ) ;
#17040 = VERTEX_POINT ( 'NONE', #5855 ) ;
#17041 = APPLICATION_CONTEXT ( 'automotive_design' ) ;
#17042 = CARTESIAN_POINT ( 'NONE',  ( 0.000000000000000000, 0.000000000000000000, -0.1559029880880275776 ) ) ;
#17043 = CARTESIAN_POINT ( 'NONE',  ( -0.09660931395005634137, -0.3606853515406420185, -3.115157480314960647 ) ) ;
#17044 = DIRECTION ( 'NONE',  ( 0.000000000000000000, 0.000000000000000000, -1.000000000000000000 ) ) ;
#17045 = CARTESIAN_POINT ( 'NONE',  ( 0.5393700787401575214, 0.000000000000000000, -3.278217716535432842E-17 ) ) ;
#17046 = LINE ( 'NONE', #27364, #19156 ) ;
#17047 = DIRECTION ( 'NONE',  ( 0.000000000000000000, 0.000000000000000000, 1.000000000000000000 ) ) ;
#17048 = ADVANCED_FACE ( 'NONE', ( #22945 ), #2683, .F. ) ;
#17049 = VECTOR ( 'NONE', #18500, 39.37007874015748143 ) ;
#17050 = FACE_OUTER_BOUND ( 'NONE', #2737, .T. ) ;
#17051 = CIRCLE ( 'NONE', #6670, 0.01377952755905510404 ) ;
#17052 = ORIENTED_EDGE ( 'NONE', *, *, #3008, .F. ) ;
#17053 = CARTESIAN_POINT ( 'NONE',  ( -0.0005789383928811193264, 0.4762008496958949344, 0.1212655228861402035 ) ) ;
#17054 = ORIENTED_EDGE ( 'NONE', *, *, #383, .F. ) ;
#17055 = ORIENTED_EDGE ( 'NONE', *, *, #7697, .F. ) ;
#17056 = VERTEX_POINT ( 'NONE', #14906 ) ;
#17057 = CARTESIAN_POINT ( 'NONE',  ( -0.1318897637674583401, 0.000000000000000000, -4.330708661396418080 ) ) ;
#17058 = PRESENTATION_STYLE_ASSIGNMENT (( #12395 ) ) ;
#17059 = CARTESIAN_POINT ( 'NONE',  ( 0.5085118447801419972, 0.06699507805369840641, 1.766732283464566899 ) ) ;
#17060 = ORIENTED_EDGE ( 'NONE', *, *, #17844, .T. ) ;
#17061 = ORIENTED_EDGE ( 'NONE', *, *, #585, .T. ) ;
#17063 = CARTESIAN_POINT ( 'NONE',  ( -0.04679574315772200288, 0.3551931031211610357, -3.115157480314960647 ) ) ;
#17062 = CARTESIAN_POINT ( 'NONE',  ( -0.07874015748031495954, -0.04546065111729338803, -0.3779527559055118058 ) ) ;
#17064 = CARTESIAN_POINT ( 'NONE',  ( 0.4561454261165569513, 0.08101060747777377724, 0.2048502514975752697 ) ) ;
#17065 = CARTESIAN_POINT ( 'NONE',  ( 0.03532354024591712049, -1.653543307086614345, 1.012503259137575512E-16 ) ) ;
#17066 = CIRCLE ( 'NONE', #2176, 0.6212598425196850238 ) ;
#17067 = CARTESIAN_POINT ( 'NONE',  ( 0.2041304421298449356, -0.2660793235464211093, 1.973425196850393970 ) ) ;
#17068 = ORIENTED_EDGE ( 'NONE', *, *, #13451, .T. ) ;
#17069 = EDGE_CURVE ( 'NONE', #11118, #16402, #23924, .T. ) ;
#17070 = VERTEX_POINT ( 'NONE', #17004 ) ;
#17071 = CARTESIAN_POINT ( 'NONE',  ( 0.3001918266902269261, 0.3912931228431901776, -1.550196850393700920 ) ) ;
#17072 = AXIS2_PLACEMENT_3D ( 'NONE', #23763, #1861, #8369 ) ;
#17073 = CARTESIAN_POINT ( 'NONE',  ( 0.5925575908939920700, 0.000000000000000000, 0.000000000000000000 ) ) ;
#17074 = ORIENTED_EDGE ( 'NONE', *, *, #20391, .F. ) ;
#17075 = ORIENTED_EDGE ( 'NONE', *, *, #6770, .F. ) ;
#17076 = ORIENTED_EDGE ( 'NONE', *, *, #8160, .F. ) ;
#17077 = FACE_OUTER_BOUND ( 'NONE', #6193, .T. ) ;
#17078 = EDGE_CURVE ( 'NONE', #20499, #16237, #3588, .T. ) ;
#17079 = CARTESIAN_POINT ( 'NONE',  ( 0.4563908000639795848, 0.9448480804523937682, -0.4282964253270322708 ) ) ;
#17080 = DIRECTION ( 'NONE',  ( 0.000000000000000000, 0.000000000000000000, 1.000000000000000000 ) ) ;
#17081 = CARTESIAN_POINT ( 'NONE',  ( 0.7165354330708662012, 0.000000000000000000, 0.01181102362204724393 ) ) ;
#17082 = VERTEX_POINT ( 'NONE', #3864 ) ;
#17083 = CARTESIAN_POINT ( 'NONE',  ( 0.5322834645669292097, 0.000000000000000000, 0.3401574803149606252 ) ) ;
#17084 = DIRECTION ( 'NONE',  ( 1.000000000000000000, 0.000000000000000000, 0.000000000000000000 ) ) ;
#17085 = DIRECTION ( 'NONE',  ( 0.000000000000000000, -1.000000000000000000, 0.000000000000000000 ) ) ;
#17086 = CARTESIAN_POINT ( 'NONE',  ( -0.6003276630397328395, -0.1991340584959632176, 0.2207559493283942353 ) ) ;
#17087 = CIRCLE ( 'NONE', #12116, 0.1181102362204718703 ) ;
#17088 = FACE_OUTER_BOUND ( 'NONE', #14625, .T. ) ;
#17089 = CIRCLE ( 'NONE', #12571, 0.1003956692913385851 ) ;
#17090 = CARTESIAN_POINT ( 'NONE',  ( -0.5190862322091315262, -0.1177929122753175184, 0.1322834645669291320 ) ) ;
#17091 = CARTESIAN_POINT ( 'NONE',  ( 0.000000000000000000, 0.5905511811023621549, 0.000000000000000000 ) ) ;
#17092 = CARTESIAN_POINT ( 'NONE',  ( -0.08600259748439828544, 0.1968503937007873850, -3.223068998490981496 ) ) ;
#17093 = VERTEX_POINT ( 'NONE', #1742 ) ;
#17094 = VECTOR ( 'NONE', #375, 39.37007874015748854 ) ;
#17095 = CARTESIAN_POINT ( 'NONE',  ( 0.1580799066051611357, -0.4326553680327475671, 0.1903859678396761790 ) ) ;
#17096 = FACE_OUTER_BOUND ( 'NONE', #26329, .T. ) ;
#17097 = EDGE_LOOP ( 'NONE', ( #25066, #27875, #16740, #20600, #9704 ) ) ;
#17098 = ORIENTED_EDGE ( 'NONE', *, *, #2158, .F. ) ;
#17099 = DIRECTION ( 'NONE',  ( 0.000000000000000000, 1.000000000000000000, 0.000000000000000000 ) ) ;
#17100 = CARTESIAN_POINT ( 'NONE',  ( 0.0007856387884297636034, 0.7354206117094393980, 0.1960773254400930421 ) ) ;
#17101 = EDGE_CURVE ( 'NONE', #26519, #8592, #23087, .T. ) ;
#17102 = CARTESIAN_POINT ( 'NONE',  ( 0.5335524835332358107, -0.1429116519061119361, 0.9202755905511811330 ) ) ;
#17103 = ORIENTED_EDGE ( 'NONE', *, *, #9683, .F. ) ;
#17104 = EDGE_CURVE ( 'NONE', #9793, #10277, #8391, .T. ) ;
#17105 = PLANE ( 'NONE',  #24342 ) ;
#17106 = ORIENTED_EDGE ( 'NONE', *, *, #18890, .T. ) ;
#17107 = VECTOR ( 'NONE', #11146, 39.37007874015748143 ) ;
#17108 = DIRECTION ( 'NONE',  ( 0.000000000000000000, 0.000000000000000000, 1.000000000000000000 ) ) ;
#17109 = CIRCLE ( 'NONE', #2668, 0.3464566929133857665 ) ;
#17110 = EDGE_CURVE ( 'NONE', #16783, #6811, #27086, .T. ) ;
#17111 = CIRCLE ( 'NONE', #425, 0.4405067310818653881 ) ;
#17112 = DIRECTION ( 'NONE',  ( 0.000000000000000000, 1.000000000000000000, 0.000000000000000000 ) ) ;
#17113 = DIRECTION ( 'NONE',  ( 0.000000000000000000, 1.000000000000000000, 0.000000000000000000 ) ) ;
#17114 = CARTESIAN_POINT ( 'NONE',  ( -0.5190862322091315262, -0.1177929122753175184, 0.1322834645669291320 ) ) ;
#17115 = EDGE_LOOP ( 'NONE', ( #4133, #10913, #5188, #11343, #21481, #1621 ) ) ;
#17116 = CARTESIAN_POINT ( 'NONE',  ( -0.1710938124795999826, -0.4706537664821763833, 0.09684793308443542803 ) ) ;
#17117 = DIRECTION ( 'NONE',  ( 1.000000000000000000, 0.000000000000000000, 0.000000000000000000 ) ) ;
#17118 = LINE ( 'NONE', #17389, #288 ) ;
#17119 = FACE_BOUND ( 'NONE', #8253, .T. ) ;
#17120 = DIRECTION ( 'NONE',  ( 0.000000000000000000, 0.000000000000000000, -1.000000000000000000 ) ) ;
#17121 = CARTESIAN_POINT ( 'NONE',  ( 0.6791338582677166613, 0.000000000000000000, 0.000000000000000000 ) ) ;
#17122 = CARTESIAN_POINT ( 'NONE',  ( 0.4382482975805209735, 0.3362148458989007715, 0.9399606299212598381 ) ) ;
#17123 = FACE_OUTER_BOUND ( 'NONE', #20679, .T. ) ;
#17124 = ORIENTED_EDGE ( 'NONE', *, *, #22693, .F. ) ;
#17125 = DIRECTION ( 'NONE',  ( 1.000000000000000000, 0.000000000000000000, 0.000000000000000000 ) ) ;
#17126 = CONICAL_SURFACE ( 'NONE', #4504, 0.5511811023975373702, 0.7853981633974482790 ) ;
#17127 = EDGE_LOOP ( 'NONE', ( #8582, #25260, #12332, #22773 ) ) ;
#17128 = ORIENTED_EDGE ( 'NONE', *, *, #25154, .F. ) ;
#17129 = ADVANCED_FACE ( 'NONE', ( #18970 ), #16872, .F. ) ;
#17130 = CARTESIAN_POINT ( 'NONE',  ( 0.1327036767636163017, -0.4954415918535808872, -1.550196850393700920 ) ) ;
#17131 = CARTESIAN_POINT ( 'NONE',  ( -0.09842519685039370636, -0.07874015748031495954, -0.04546065111729338803 ) ) ;
#17132 = CARTESIAN_POINT ( 'NONE',  ( 0.000000000000000000, 0.000000000000000000, -0.2480314960629921295 ) ) ;
#17133 = FACE_BOUND ( 'NONE', #13481, .T. ) ;
#17134 = CARTESIAN_POINT ( 'NONE',  ( 0.1711665596932999966, -0.5043892184459949357, 1.747047244094488194 ) ) ;
#17135 = EDGE_CURVE ( 'NONE', #4605, #20543, #18487, .T. ) ;
#17136 = DIRECTION ( 'NONE',  ( 0.000000000000000000, 0.000000000000000000, -1.000000000000000000 ) ) ;
#17137 = ORIENTED_EDGE ( 'NONE', *, *, #26321, .F. ) ;
#17138 = CARTESIAN_POINT ( 'NONE',  ( 0.000000000000000000, 0.000000000000000000, 0.2374015748031496065 ) ) ;
#17139 = DIRECTION ( 'NONE',  ( 1.000000000000000000, 0.000000000000000000, 0.000000000000000000 ) ) ;
#17140 = CARTESIAN_POINT ( 'NONE',  ( 0.3988311005573134116, 0.4763376377694984454, 0.09685039370078740717 ) ) ;
#17141 = CARTESIAN_POINT ( 'NONE',  ( 0.1599629598573824862, -0.4411872753631803090, 0.07637795275590551769 ) ) ;
#17142 = ORIENTED_EDGE ( 'NONE', *, *, #25931, .T. ) ;
#17143 = AXIS2_PLACEMENT_3D ( 'NONE', #23412, #12371, #6306 ) ;
#17144 = AXIS2_PLACEMENT_3D ( 'NONE', #21319, #12559, #21176 ) ;
#17145 = FACE_OUTER_BOUND ( 'NONE', #27037, .T. ) ;
#17146 = CARTESIAN_POINT ( 'NONE',  ( -0.2303471512294322787, -0.4798602677570401598, 0.1322834645669291320 ) ) ;
#17147 = DIRECTION ( 'NONE',  ( 0.000000000000000000, 1.000000000000000000, 0.000000000000000000 ) ) ;
#17148 = VERTEX_POINT ( 'NONE', #5996 ) ;
#17149 = DIRECTION ( 'NONE',  ( -1.000000000000000000, 0.000000000000000000, 0.000000000000000000 ) ) ;
#17150 = B_SPLINE_CURVE_WITH_KNOTS ( 'NONE', 3,
 ( #11752, #24455, #20232, #26720, #16001, #13877 ),
 .UNSPECIFIED., .F., .F.,
 ( 4, 2, 4 ),
 ( 0.000000000000000000, 0.2500000000000000000, 0.5000000000000000000 ),
 .UNSPECIFIED. ) ;
#17151 = CARTESIAN_POINT ( 'NONE',  ( -0.3912931228432153796, -0.3001918266902245391, -1.569881889763779625 ) ) ;
#17152 = EDGE_CURVE ( 'NONE', #26179, #4298, #13531, .T. ) ;
#17153 = CARTESIAN_POINT ( 'NONE',  ( -0.1458850421962410715, 0.4296318976989903504, -1.934055118110236338 ) ) ;
#17154 = CIRCLE ( 'NONE', #3663, 0.01181102362204724046 ) ;
#17155 = CARTESIAN_POINT ( 'NONE',  ( 0.1610509776512594748, -0.4407912692718567449, 0.1992125984251968684 ) ) ;
#17156 = DIRECTION ( 'NONE',  ( -1.000000000000000000, -1.224646799147353454E-16, 0.000000000000000000 ) ) ;
#17157 = EDGE_LOOP ( 'NONE', ( #26021, #13829, #2689, #1790 ) ) ;
#17158 = CARTESIAN_POINT ( 'NONE',  ( -0.5632721120450597807, -0.2893425403402185014, 0.04127604646039393504 ) ) ;
#17159 = DIRECTION ( 'NONE',  ( 0.000000000000000000, 0.000000000000000000, 1.000000000000000000 ) ) ;
#17160 = DIRECTION ( 'NONE',  ( -1.000000000000000000, 0.000000000000000000, 0.000000000000000000 ) ) ;
#17161 = ORIENTED_EDGE ( 'NONE', *, *, #11134, .F. ) ;
#17162 = AXIS2_PLACEMENT_3D ( 'NONE', #22553, #24520, #3035 ) ;
#17163 = DIRECTION ( 'NONE',  ( -1.000000000000000000, 0.000000000000000000, 0.000000000000000000 ) ) ;
#17164 = CARTESIAN_POINT ( 'NONE',  ( -0.3429848536917952662, -0.09193072188233032682, 1.953740157480315043 ) ) ;
#17165 = CARTESIAN_POINT ( 'NONE',  ( 0.4055118110236220486, 0.000000000000000000, 0.01181102362204724393 ) ) ;
#17166 = CARTESIAN_POINT ( 'NONE',  ( -0.1431849087158744982, 0.4219262446672297773, -1.934055118110236116 ) ) ;
#17167 = EDGE_CURVE ( 'NONE', #7189, #8124, #20330, .T. ) ;
#17168 = ORIENTED_EDGE ( 'NONE', *, *, #26852, .T. ) ;
#17169 = CARTESIAN_POINT ( 'NONE',  ( -0.04638120790932924453, 0.3520466617657084796, 1.953740157480315043 ) ) ;
#17170 = ORIENTED_EDGE ( 'NONE', *, *, #9171, .T. ) ;
#17171 = CARTESIAN_POINT ( 'NONE',  ( -0.4218945342797526532, -0.1432577568504610210, -1.934055118110236338 ) ) ;
#17172 = MECHANICAL_DESIGN_GEOMETRIC_PRESENTATION_REPRESENTATION (  '', ( #2279 ), #956 ) ;
#17173 = CARTESIAN_POINT ( 'NONE',  ( -0.6099157123460891006, -0.1048986197189705483, -0.2429871477880080621 ) ) ;
#17174 = CARTESIAN_POINT ( 'NONE',  ( -0.5484420430269733027, -0.3174147232946766817, 0.1061598535666647691 ) ) ;
#17175 = CARTESIAN_POINT ( 'NONE',  ( -0.4954156765914849991, -0.2860899518037616773, 0.9399606299212598381 ) ) ;
#17176 = CARTESIAN_POINT ( 'NONE',  ( 0.3334645669291338987, -0.9395870660861969093, -0.7720950382133976442 ) ) ;
#17177 = DIRECTION ( 'NONE',  ( 0.000000000000000000, 0.000000000000000000, 1.000000000000000000 ) ) ;
#17178 = CARTESIAN_POINT ( 'NONE',  ( 0.3535721684717935132, 0.1200583359873110406, -3.115157480314960647 ) ) ;
#17179 = CARTESIAN_POINT ( 'NONE',  ( 0.5525004126151165096, 0.09742072959660433296, 0.1771653543307086520 ) ) ;
#17180 = CARTESIAN_POINT ( 'NONE',  ( -0.2362204724409449064, 0.9448818897637796255, -9.561468503937007847E-18 ) ) ;
#17181 = CARTESIAN_POINT ( 'NONE',  ( 0.003937007874015826907, -4.393043307086613241E-18, 0.000000000000000000 ) ) ;
#17182 = DIRECTION ( 'NONE',  ( -0.000000000000000000, -1.000000000000000000, -0.000000000000000000 ) ) ;
#17183 = EDGE_CURVE ( 'NONE', #1325, #8592, #6346, .T. ) ;
#17184 = DIRECTION ( 'NONE',  ( 0.000000000000000000, 0.000000000000000000, 1.000000000000000000 ) ) ;
#17185 = AXIS2_PLACEMENT_3D ( 'NONE', #17873, #26366, #13506 ) ;
#17186 = CARTESIAN_POINT ( 'NONE',  ( 0.7430739993161732393, 0.4449930158387386259, -0.3601246575843464748 ) ) ;
#17187 = VERTEX_POINT ( 'NONE', #10072 ) ;
#17188 = CARTESIAN_POINT ( 'NONE',  ( 6.991093932464927839E-17, 0.03937007874015751446, -0.5511811023975373702 ) ) ;
#17189 = ORIENTED_EDGE ( 'NONE', *, *, #23042, .T. ) ;
#17190 = VERTEX_POINT ( 'NONE', #27319 ) ;
#17191 = CARTESIAN_POINT ( 'NONE',  ( -1.197070535079588716, 0.07874015748031495954, -1.078960298859116707 ) ) ;
#17192 = CARTESIAN_POINT ( 'NONE',  ( 0.4932821129636645874, 0.08637579872942321990, 0.09685039370078740717 ) ) ;
#17193 = CARTESIAN_POINT ( 'NONE',  ( 0.3855916753051394363, 0.3382184156732163660, 1.766732283464566899 ) ) ;
#17194 = CARTESIAN_POINT ( 'NONE',  ( -0.4954415918530866159, 0.1327036767659691974, 1.747047244094488194 ) ) ;
#17195 = DIRECTION ( 'NONE',  ( 0.000000000000000000, 0.000000000000000000, -1.000000000000000000 ) ) ;
#17196 = ORIENTED_EDGE ( 'NONE', *, *, #11342, .F. ) ;
#17198 = CARTESIAN_POINT ( 'NONE',  ( 0.1791601451668926592, -0.3102476824511484210, -3.115157480314960647 ) ) ;
#17197 = DIRECTION ( 'NONE',  ( -0.9790454724845842893, -0.1018208755700880375, -0.1763589297585410332 ) ) ;
#17199 = VERTEX_POINT ( 'NONE', #14480 ) ;
#17200 = CARTESIAN_POINT ( 'NONE',  ( -0.1632039128451868437, -0.4501088385448056006, 0.1920935997054097066 ) ) ;
#17201 = B_SPLINE_CURVE_WITH_KNOTS ( 'NONE', 3,
 ( #27190, #12484, #5718, #10077, #23385, #25056 ),
 .UNSPECIFIED., .F., .F.,
 ( 4, 2, 4 ),
 ( 0.9359046326923009529, 0.9375808709372039917, 0.9392571091821080298 ),
 .UNSPECIFIED. ) ;
#17202 = CARTESIAN_POINT ( 'NONE',  ( 0.3339160553493882300, 0.7867001919223544082, -0.8344257386302499357 ) ) ;
#17203 = ADVANCED_FACE ( 'NONE', ( #12336, #1600 ), #23231, .T. ) ;
#17204 = CARTESIAN_POINT ( 'NONE',  ( -0.1078280746904044657, 0.3175540113612282389, 1.973425196850393970 ) ) ;
#17205 = ORIENTED_EDGE ( 'NONE', *, *, #18848, .F. ) ;
#17206 = VERTEX_POINT ( 'NONE', #14775 ) ;
#17207 = EDGE_CURVE ( 'NONE', #22691, #14646, #17593, .T. ) ;
#17208 = CONICAL_SURFACE ( 'NONE', #22150, 0.4307823082429378392, 0.9572651268756555698 ) ;
#17209 = LINE ( 'NONE', #14561, #13833 ) ;
#17210 = DIRECTION ( 'NONE',  ( -1.000000000000000000, 0.000000000000000000, 0.000000000000000000 ) ) ;
#17211 = ORIENTED_EDGE ( 'NONE', *, *, #27831, .F. ) ;
#17212 = ORIENTED_EDGE ( 'NONE', *, *, #2233, .T. ) ;
#17213 = ORIENTED_EDGE ( 'NONE', *, *, #9722, .T. ) ;
#17214 = DIRECTION ( 'NONE',  ( 0.000000000000000000, 0.000000000000000000, -1.000000000000000000 ) ) ;
#17215 = AXIS2_PLACEMENT_3D ( 'NONE', #5449, #11653, #9520 ) ;
#17216 = DIRECTION ( 'NONE',  ( 0.000000000000000000, 0.000000000000000000, -1.000000000000000000 ) ) ;
#17217 = DIRECTION ( 'NONE',  ( 0.4338837391175581759, -0.9009688679024190350, 0.000000000000000000 ) ) ;
#17218 = DIRECTION ( 'NONE',  ( 0.000000000000000000, 1.000000000000000000, 0.000000000000000000 ) ) ;
#17219 = ORIENTED_EDGE ( 'NONE', *, *, #18548, .F. ) ;
#17220 = DIRECTION ( 'NONE',  ( 0.000000000000000000, 0.000000000000000000, 1.000000000000000000 ) ) ;
#17221 = CONTEXT_DEPENDENT_SHAPE_REPRESENTATION ( #4416, #11173 ) ;
#17222 = CARTESIAN_POINT ( 'NONE',  ( -0.05118110236220472370, 0.000000000000000000, 0.000000000000000000 ) ) ;
#17223 = EDGE_CURVE ( 'NONE', #16511, #21309, #27095, .T. ) ;
#17224 = CARTESIAN_POINT ( 'NONE',  ( -0.4351030398461813720, -0.1477428134820238381, -1.928289503579156294 ) ) ;
#17225 = AXIS2_PLACEMENT_3D ( 'NONE', #8523, #444, #26138 ) ;
#17226 = CARTESIAN_POINT ( 'NONE',  ( 0.1522836969735573143, 0.2938892803217905692, 0.3971963147566898167 ) ) ;
#17227 = CARTESIAN_POINT ( 'NONE',  ( 0.4300129863948118913, 0.2478439864030018147, -1.569881889763779403 ) ) ;
#17228 = FACE_OUTER_BOUND ( 'NONE', #14431, .T. ) ;
#17229 = AXIS2_PLACEMENT_3D ( 'NONE', #26185, #8675, #25915 ) ;
#17230 = B_SPLINE_CURVE_WITH_KNOTS ( 'NONE', 3,
 ( #738, #20223, #22625, #5535, #17935, #26707, #5243, #14158, #7224, #26855, #15988, #16135, #22155, #11014, #13125, #691, #24274, #21893 ),
 .UNSPECIFIED., .F., .F.,
 ( 4, 2, 2, 2, 2, 2, 2, 2, 4 ),
 ( 0.5000000000000000000, 0.5625000000000000000, 0.6250000000000001110, 0.6875000000000001110, 0.7500000000000001110, 0.8125000000000001110, 0.8750000000000000000, 0.9375000000000000000, 1.000000000000000000 ),
 .UNSPECIFIED. ) ;
#17231 = CARTESIAN_POINT ( 'NONE',  ( 0.1525037638700916243, 0.2637554987713724985, 0.4194810972668291393 ) ) ;
#17232 = ORIENTED_EDGE ( 'NONE', *, *, #675, .F. ) ;
#17233 = EDGE_CURVE ( 'NONE', #9309, #22865, #5421, .T. ) ;
#17234 = ORIENTED_EDGE ( 'NONE', *, *, #16578, .T. ) ;
#17235 = LINE ( 'NONE', #25432, #27439 ) ;
#17236 = ( CONVERSION_BASED_UNIT ( 'INCH', #1839 ) LENGTH_UNIT ( ) NAMED_UNIT ( #25859 ) ) ;
#17237 = ORIENTED_EDGE ( 'NONE', *, *, #5885, .T. ) ;
#17238 = FACE_OUTER_BOUND ( 'NONE', #19909, .T. ) ;
#17239 = CARTESIAN_POINT ( 'NONE',  ( 0.000000000000000000, 0.3937007873309092409, 0.000000000000000000 ) ) ;
#17240 = ORIENTED_EDGE ( 'NONE', *, *, #19523, .T. ) ;
#17241 = CARTESIAN_POINT ( 'NONE',  ( 0.2442565704126255510, -0.4954197419817655823, 0.9202755905511811330 ) ) ;
#17242 = DIRECTION ( 'NONE',  ( 0.000000000000000000, 1.000000000000000000, 0.000000000000000000 ) ) ;
#17243 = ORIENTED_EDGE ( 'NONE', *, *, #81, .F. ) ;
#17244 = CARTESIAN_POINT ( 'NONE',  ( -0.4339912984563299436, -0.2498791196563492356, 0.09685039370078740717 ) ) ;
#17245 = CARTESIAN_POINT ( 'NONE',  ( 0.2428345617565153547, 0.2885915454824177218, 0.07637795275590551769 ) ) ;
#17246 = AXIS2_PLACEMENT_3D ( 'NONE', #17248, #26140, #24018 ) ;
#17247 = CARTESIAN_POINT ( 'NONE',  ( 0.1506723201675407575, 0.000000000000000000, 0.000000000000000000 ) ) ;
#17248 = CARTESIAN_POINT ( 'NONE',  ( 0.000000000000000000, 0.000000000000000000, 0.000000000000000000 ) ) ;
#17249 = ORIENTED_EDGE ( 'NONE', *, *, #23921, .F. ) ;
#17250 = CARTESIAN_POINT ( 'NONE',  ( -0.5021077788545322829, -0.1139291307079571824, 0.1473214333301098022 ) ) ;
#17251 = AXIS2_PLACEMENT_3D ( 'NONE', #25237, #14530, #7736 ) ;
#17252 = ( BOUNDED_CURVE ( )  B_SPLINE_CURVE ( 3, ( #11614, #3263, #7671, #16288 ),
 .UNSPECIFIED., .F., .T. ) 
 B_SPLINE_CURVE_WITH_KNOTS ( ( 4, 4 ),
 ( 3.141592653589793116, 3.254758905499643973 ),
 .UNSPECIFIED. ) 
 CURVE ( )  GEOMETRIC_REPRESENTATION_ITEM ( )  RATIONAL_B_SPLINE_CURVE ( ( 1.000000000000000000, 0.9989330679932157953, 0.9989330679932157953, 1.000000000000000000 ) ) 
 REPRESENTATION_ITEM ( '' )  ) ;
#17253 = DIRECTION ( 'NONE',  ( -0.4999999999999995004, 0.8660254037844390407, 0.000000000000000000 ) ) ;
#17254 = DIRECTION ( 'NONE',  ( 0.000000000000000000, 0.000000000000000000, -1.000000000000000000 ) ) ;
#17255 = CARTESIAN_POINT ( 'NONE',  ( 0.4622619257814448712, 0.08092139668561752763, 0.1992125984251968684 ) ) ;
#17256 = CARTESIAN_POINT ( 'NONE',  ( 0.003937007874015826907, -4.393043307086613241E-18, 0.000000000000000000 ) ) ;
#17257 = TOROIDAL_SURFACE ( 'NONE', #24445, 0.6102362204724409711, 0.1299212598425196763 ) ;
#17258 = CARTESIAN_POINT ( 'NONE',  ( -0.06200787401574806706, 7.593774443531820041E-18, 0.7844728274238290666 ) ) ;
#17259 = CARTESIAN_POINT ( 'NONE',  ( 0.03532354024591842501, -0.6299212598425196763, 0.000000000000000000 ) ) ;
#17260 = EDGE_CURVE ( 'NONE', #2756, #20128, #19538, .T. ) ;
#17261 = CARTESIAN_POINT ( 'NONE',  ( 0.4954156765914486393, 0.2860899518037346989, 0.9399606299212598381 ) ) ;
#17262 = CARTESIAN_POINT ( 'NONE',  ( 0.1522836969735573143, 0.000000000000000000, 0.000000000000000000 ) ) ;
#17264 = CARTESIAN_POINT ( 'NONE',  ( 4.821444091131312140E-17, 0.1968503937007874127, 0.3937007874015748254 ) ) ;
#17265 = EDGE_CURVE ( 'NONE', #26289, #7632, #24809, .T. ) ;
#17266 = CIRCLE ( 'NONE', #1027, 1.377952755905512472 ) ;
#17267 = AXIS2_PLACEMENT_3D ( 'NONE', #14881, #8489, #17113 ) ;
#17268 = EDGE_CURVE ( 'NONE', #26549, #23101, #19335, .T. ) ;
#17269 = DIRECTION ( 'NONE',  ( 1.000000000000000000, 0.000000000000000000, 0.000000000000000000 ) ) ;
#17270 = EDGE_LOOP ( 'NONE', ( #12133, #25352, #11525, #11668 ) ) ;
#17271 = CARTESIAN_POINT ( 'NONE',  ( -0.07462150385364368921, -0.5672083774005965973, 0.9399606299212601712 ) ) ;
#17272 = DIRECTION ( 'NONE',  ( 0.2588190448135640476, 3.169619147893065576E-17, -0.9659258263664939337 ) ) ;
#17273 = DIRECTION ( 'NONE',  ( 1.000000000000000000, 0.000000000000000000, 0.000000000000000000 ) ) ;
#17274 = CARTESIAN_POINT ( 'NONE',  ( 0.4681308612729627727, -0.1074986424507606286, 0.2362204724409450174 ) ) ;
#17275 = VERTEX_POINT ( 'NONE', #23653 ) ;
#17276 = CARTESIAN_POINT ( 'NONE',  ( -0.3169330146481601496, -0.1835719822042344573, 0.1910323753027497184 ) ) ;
#17277 = EDGE_LOOP ( 'NONE', ( #23753, #942 ) ) ;
#17278 = DIRECTION ( 'NONE',  ( -0.000000000000000000, -0.000000000000000000, 1.000000000000000000 ) ) ;
#17279 = DIRECTION ( 'NONE',  ( 0.000000000000000000, 1.000000000000000000, 0.000000000000000000 ) ) ;
#17280 = DIRECTION ( 'NONE',  ( -0.2036417511401759362, -0.4895227362422912565, 0.8478782506317890100 ) ) ;
#17281 = DIRECTION ( 'NONE',  ( 0.000000000000000000, 0.000000000000000000, 1.000000000000000000 ) ) ;
#17282 = EDGE_CURVE ( 'NONE', #22329, #17815, #24146, .T. ) ;
#17283 = CONICAL_SURFACE ( 'NONE', #17706, 0.1106489370078740930, 0.08726646250000029414 ) ;
#17284 = LINE ( 'NONE', #13440, #24951 ) ;
#17285 = VERTEX_POINT ( 'NONE', #9062 ) ;
#17286 = CARTESIAN_POINT ( 'NONE',  ( -0.4622619257814346572, 0.08092139668567638333, 0.07637795275590551769 ) ) ;
#17287 = CARTESIAN_POINT ( 'NONE',  ( 0.4498374011142918794, -0.05926487674658236643, -1.934055118110236338 ) ) ;
#17288 = EDGE_CURVE ( 'NONE', #23446, #12969, #470, .T. ) ;
#17289 = EDGE_CURVE ( 'NONE', #26710, #11052, #1468, .T. ) ;
#17290 = CARTESIAN_POINT ( 'NONE',  ( -1.197070535079588716, 0.4724409448818898127, 1.197070535079588716 ) ) ;
#17291 = EDGE_CURVE ( 'NONE', #21258, #13825, #8870, .T. ) ;
#17292 = CARTESIAN_POINT ( 'NONE',  ( -0.6370261810203012853, -0.06082699205827991895, 0.07717020748573424904 ) ) ;
#17293 = CONTEXT_DEPENDENT_SHAPE_REPRESENTATION ( #15073, #13889 ) ;
#17294 = CIRCLE ( 'NONE', #20909, 0.5322834645669292097 ) ;
#17295 = ORIENTED_EDGE ( 'NONE', *, *, #9482, .F. ) ;
#17296 = AXIS2_PLACEMENT_3D ( 'NONE', #15844, #24319, #9194 ) ;
#17297 = CARTESIAN_POINT ( 'NONE',  ( 0.000000000000000000, 0.000000000000000000, 0.1322834645669291320 ) ) ;
#17298 = DIRECTION ( 'NONE',  ( 0.000000000000000000, -1.000000000000000000, 0.000000000000000000 ) ) ;
#17299 = DIRECTION ( 'NONE',  ( 0.000000000000000000, 0.000000000000000000, 1.000000000000000000 ) ) ;
#17300 = AXIS2_PLACEMENT_3D ( 'NONE', #18168, #27105, #26661 ) ;
#17301 = CARTESIAN_POINT ( 'NONE',  ( 0.1970998888482821121, 0.3995939286813822711, -1.934055118110236560 ) ) ;
#17302 = CARTESIAN_POINT ( 'NONE',  ( -0.6722178168900768691, 0.04410929521222984456, -0.07961573540161062668 ) ) ;
#17303 = ORIENTED_EDGE ( 'NONE', *, *, #11181, .T. ) ;
#17304 = CIRCLE ( 'NONE', #21388, 0.8267716535433071723 ) ;
#17305 = CARTESIAN_POINT ( 'NONE',  ( -0.3411003281196917092, 0.2991932138496784521, -1.934055118110236338 ) ) ;
#17306 = CARTESIAN_POINT ( 'NONE',  ( 0.1518453844022533417, 0.1971119370939669324, -0.4530813475038473204 ) ) ;
#17307 = CARTESIAN_POINT ( 'NONE',  ( 0.000000000000000000, 0.000000000000000000, -0.1309055118110236116 ) ) ;
#17308 = CARTESIAN_POINT ( 'NONE',  ( 0.5708661417322835607, 0.03736310157557569400, 0.9399606299212598381 ) ) ;
#17309 = AXIS2_PLACEMENT_3D ( 'NONE', #39, #4232, #2511 ) ;
#17310 = VERTEX_POINT ( 'NONE', #2163 ) ;
#17311 = FACE_BOUND ( 'NONE', #24518, .T. ) ;
#17312 = ORIENTED_EDGE ( 'NONE', *, *, #15862, .T. ) ;
#17313 = FACE_BOUND ( 'NONE', #4880, .T. ) ;
#17314 = CARTESIAN_POINT ( 'NONE',  ( 0.2227473777839351354, -0.3858850602360253679, -1.934055118110236560 ) ) ;
#17315 = DIRECTION ( 'NONE',  ( 0.000000000000000000, 1.000000000000000000, 0.000000000000000000 ) ) ;
#17316 = DIRECTION ( 'NONE',  ( 0.000000000000000000, 0.000000000000000000, -1.000000000000000000 ) ) ;
#17317 = DIRECTION ( 'NONE',  ( 1.000000000000000000, 0.000000000000000000, 0.000000000000000000 ) ) ;
#17318 = CARTESIAN_POINT ( 'NONE',  ( 8.353478384051541640E-17, -4.420672499999999463E-18, -0.1023622047244094474 ) ) ;
#17319 = TOROIDAL_SURFACE ( 'NONE', #5117, 0.7165354330708662012, 0.01181102362204724393 ) ;
#17320 = ORIENTED_EDGE ( 'NONE', *, *, #24972, .T. ) ;
#17321 = CARTESIAN_POINT ( 'NONE',  ( -0.6118597084614586512, 0.1076640027107653580, 0.2574827755769819038 ) ) ;
#17322 = ADVANCED_FACE ( 'NONE', ( #8791 ), #16256, .F. ) ;
#17323 = ADVANCED_FACE ( 'NONE', ( #15324 ), #91, .T. ) ;
#17324 = FACE_OUTER_BOUND ( 'NONE', #14257, .T. ) ;
#17325 = AXIS2_PLACEMENT_3D ( 'NONE', #6673, #17796, #9310 ) ;
#17326 = ORIENTED_EDGE ( 'NONE', *, *, #4823, .F. ) ;
#17327 = AXIS2_PLACEMENT_3D ( 'NONE', #13306, #17273, #14439 ) ;
#17328 = VERTEX_POINT ( 'NONE', #4430 ) ;
#17329 = B_SPLINE_CURVE_WITH_KNOTS ( 'NONE', 3,
 ( #10440, #22112, #13484, #8340, #25703, #23329, #21470, #10728, #10294, #2239, #16953, #6088, #21608, #15260, #25569, #10860, #4095, #12701 ),
 .UNSPECIFIED., .F., .F.,
 ( 4, 2, 2, 2, 2, 2, 2, 2, 4 ),
 ( 0.5000000000000000000, 0.5625000000000000000, 0.6250000000000000000, 0.6875000000000000000, 0.7500000000000000000, 0.8125000000000000000, 0.8750000000000000000, 0.9375000000000000000, 1.000000000000000000 ),
 .UNSPECIFIED. ) ;
#17330 = CARTESIAN_POINT ( 'NONE',  ( 0.000000000000000000, 0.000000000000000000, -2.322834645648386154 ) ) ;
#17331 = APPLICATION_PROTOCOL_DEFINITION ( 'draft international standard', 'automotive_design', 1998, #21908 ) ;
#17332 = CARTESIAN_POINT ( 'NONE',  ( 0.4069448477556011912, 0.3121994997598430133, 1.766732283464566899 ) ) ;
#17333 = ADVANCED_FACE ( 'NONE', ( #13035 ), #25614, .T. ) ;
#17334 = SURFACE_STYLE_FILL_AREA ( #2616 ) ;
#17335 = VERTEX_POINT ( 'NONE', #13163 ) ;
#17336 = ORIENTED_EDGE ( 'NONE', *, *, #20971, .T. ) ;
#17338 = CARTESIAN_POINT ( 'NONE',  ( -0.3213305936751578717, -0.1584254766472200371, -3.115157480314960647 ) ) ;
#17337 = PLANE ( 'NONE',  #24706 ) ;
#17339 = ORIENTED_EDGE ( 'NONE', *, *, #27470, .T. ) ;
#17340 = ORIENTED_EDGE ( 'NONE', *, *, #10914, .T. ) ;
#17341 = DIRECTION ( 'NONE',  ( -0.2036417511401759084, 0.4895227362422917006, -0.8478782506317888989 ) ) ;
#17342 = SPHERICAL_SURFACE ( 'NONE', #14087, 0.1003956692913385851 ) ;
#17343 = AXIS2_PLACEMENT_3D ( 'NONE', #17914, #15570, #11172 ) ;
#17344 = CARTESIAN_POINT ( 'NONE',  ( -0.1482986320106521871, -0.3007905576423956506, 1.953740157480315043 ) ) ;
#17345 = VERTEX_POINT ( 'NONE', #21793 ) ;
#17346 = ORIENTED_EDGE ( 'NONE', *, *, #27426, .F. ) ;
#17347 = CARTESIAN_POINT ( 'NONE',  ( 0.1522836969735571200, -0.4941010236220468865, -0.01864847287710779539 ) ) ;
#17348 = DIRECTION ( 'NONE',  ( 1.000000000000000000, 0.000000000000000000, 0.000000000000000000 ) ) ;
#17349 = ORIENTED_EDGE ( 'NONE', *, *, #23027, .T. ) ;
#17350 = EDGE_LOOP ( 'NONE', ( #25036, #2822, #12550, #21495 ) ) ;
#17351 = ORIENTED_EDGE ( 'NONE', *, *, #14410, .T. ) ;
#17352 = VECTOR ( 'NONE', #3813, 39.37007874015748854 ) ;
#17353 = DIRECTION ( 'NONE',  ( 1.000000000000000000, 0.000000000000000000, 0.000000000000000000 ) ) ;
#17354 = CIRCLE ( 'NONE', #24547, 0.4405067310818653881 ) ;
#17355 = CARTESIAN_POINT ( 'NONE',  ( 0.1287090038540882331, -0.1704774416898503786, -0.09842519685039387289 ) ) ;
#17356 = LINE ( 'NONE', #4623, #10120 ) ;
#17357 = ORIENTED_EDGE ( 'NONE', *, *, #12765, .T. ) ;
#17358 = EDGE_CURVE ( 'NONE', #3406, #1472, #808, .T. ) ;
#17359 = DIRECTION ( 'NONE',  ( -0.000000000000000000, -0.000000000000000000, 1.000000000000000000 ) ) ;
#17360 = EDGE_CURVE ( 'NONE', #24281, #6591, #12028, .T. ) ;
#17361 = CIRCLE ( 'NONE', #5158, 0.5379714048901780288 ) ;
#17362 = CARTESIAN_POINT ( 'NONE',  ( 0.1493402947442836470, -0.2564861316490620879, 0.4057730592017521065 ) ) ;
#17363 = EDGE_CURVE ( 'NONE', #23405, #11020, #2461, .T. ) ;
#17364 = CARTESIAN_POINT ( 'NONE',  ( -0.3622090647521423734, -1.108209299994242114, -0.3946014861199982349 ) ) ;
#17365 = DIRECTION ( 'NONE',  ( 0.000000000000000000, 0.000000000000000000, -1.000000000000000000 ) ) ;
#17366 = CARTESIAN_POINT ( 'NONE',  ( -0.5188388941967637669, -0.1188778293835246053, 0.1322818204150990051 ) ) ;
#17367 = DIRECTION ( 'NONE',  ( 1.000000000000000000, 0.000000000000000000, -0.000000000000000000 ) ) ;
#17368 = AXIS2_PLACEMENT_3D ( 'NONE', #2405, #6523, #19661 ) ;
#17369 = CARTESIAN_POINT ( 'NONE',  ( 0.06296589279854367116, 0.1968503937007873850, -3.224248289462122941 ) ) ;
#17370 = VERTEX_POINT ( 'NONE', #3242 ) ;
#17371 = CIRCLE ( 'NONE', #6115, 0.3740157480314960647 ) ;
#17372 = CARTESIAN_POINT ( 'NONE',  ( 0.3937007874015748254, 0.000000000000000000, -3.115157480314960647 ) ) ;
#17373 = VERTEX_POINT ( 'NONE', #20362 ) ;
#17374 = CARTESIAN_POINT ( 'NONE',  ( 0.09842519685039370636, 0.2991866959364303802, -3.272637795275590733 ) ) ;
#17375 = DIRECTION ( 'NONE',  ( 0.000000000000000000, -1.000000000000000000, 0.000000000000000000 ) ) ;
#17376 = CARTESIAN_POINT ( 'NONE',  ( 0.000000000000000000, 0.000000000000000000, 0.09685039370078740717 ) ) ;
#17377 = CARTESIAN_POINT ( 'NONE',  ( 0.0007683673430012761965, 0.7042519390037932370, 0.3281099440175705984 ) ) ;
#17378 = VERTEX_POINT ( 'NONE', #15712 ) ;
#17379 = CARTESIAN_POINT ( 'NONE',  ( -0.4152525734086447429, -0.3642352168757386210, 0.9202755905511811330 ) ) ;
#17380 = ORIENTED_EDGE ( 'NONE', *, *, #19297, .T. ) ;
#17381 = VERTEX_POINT ( 'NONE', #24314 ) ;
#17382 = CARTESIAN_POINT ( 'NONE',  ( 1.877524803149606209E-16, 0.000000000000000000, 0.000000000000000000 ) ) ;
#17383 = DIRECTION ( 'NONE',  ( 1.000000000000000000, 0.000000000000000000, 0.000000000000000000 ) ) ;
#17384 = CARTESIAN_POINT ( 'NONE',  ( 0.4158785340170984557, 0.3322209827720822850, 0.1322818204150988386 ) ) ;
#17385 = CARTESIAN_POINT ( 'NONE',  ( -0.3665264996331779601, -0.2116141732283464416, 0.06102165354330708891 ) ) ;
#17386 = DIRECTION ( 'NONE',  ( 1.000000000000000000, 0.000000000000000000, 0.000000000000000000 ) ) ;
#17387 = TOROIDAL_SURFACE ( 'NONE', #5189, 0.5610236220472440971, 0.1003937007874015908 ) ;
#17388 = DIRECTION ( 'NONE',  ( 1.000000000000000000, 0.000000000000000000, 0.000000000000000000 ) ) ;
#17389 = CARTESIAN_POINT ( 'NONE',  ( 0.3339160553493877859, 5.862181872755905604E-06, -1.869015748010449007 ) ) ;
#17390 = FACE_OUTER_BOUND ( 'NONE', #24275, .T. ) ;
#17391 = VECTOR ( 'NONE', #10465, 39.37007874015748143 ) ;
#17392 = FACE_OUTER_BOUND ( 'NONE', #27114, .T. ) ;
#17393 = ADVANCED_FACE ( 'NONE', ( #20502 ), #5291, .F. ) ;
#17394 = CARTESIAN_POINT ( 'NONE',  ( 0.6106000000000000316, -0.09842519683305382683, 0.000000000000000000 ) ) ;
#17395 = CARTESIAN_POINT ( 'NONE',  ( 0.5708661417322835607, -0.03736310157557555522, 0.9399606299212598381 ) ) ;
#17396 = DIRECTION ( 'NONE',  ( 0.000000000000000000, -1.000000000000000000, 0.000000000000000000 ) ) ;
#17397 = VERTEX_POINT ( 'NONE', #735 ) ;
#17398 = CARTESIAN_POINT ( 'NONE',  ( 0.3224687058348476576, 3.949102684258356242E-17, -0.1559029880880275776 ) ) ;
#17399 = DIRECTION ( 'NONE',  ( 0.000000000000000000, 0.000000000000000000, 1.000000000000000000 ) ) ;
#17400 = AXIS2_PLACEMENT_3D ( 'NONE', #12176, #6776, #4101 ) ;
#17401 = EDGE_LOOP ( 'NONE', ( #5867, #15539, #15100, #22644 ) ) ;
#17402 = ORIENTED_EDGE ( 'NONE', *, *, #13370, .T. ) ;
#17403 = AXIS2_PLACEMENT_3D ( 'NONE', #18038, #3218, #26827 ) ;
#17404 = DIRECTION ( 'NONE',  ( -1.000000000000000000, 0.000000000000000000, 0.000000000000000000 ) ) ;
#17405 = CARTESIAN_POINT ( 'NONE',  ( 0.000000000000000000, 0.000000000000000000, -0.2342519685039370358 ) ) ;
#17406 = CARTESIAN_POINT ( 'NONE',  ( -0.2647715730835492609, -0.5498038367121063086, 0.2362204724409449064 ) ) ;
#17407 = ADVANCED_FACE ( 'NONE', ( #5392 ), #21092, .T. ) ;
#17408 = ORIENTED_EDGE ( 'NONE', *, *, #9644, .T. ) ;
#17409 = AXIS2_PLACEMENT_3D ( 'NONE', #25643, #10516, #17031 ) ;
#17410 = PRODUCT_DEFINITION ( 'UNKNOWN', '', #10661, #9664 ) ;
#17411 = CARTESIAN_POINT ( 'NONE',  ( 0.07614184848677874040, 0.000000000000000000, 0.000000000000000000 ) ) ;
#17412 = EDGE_CURVE ( 'NONE', #18929, #8838, #22436, .T. ) ;
#17413 = CARTESIAN_POINT ( 'NONE',  ( -0.4335958738490826581, -0.2505647196907692664, 0.2574827755769819038 ) ) ;
#17414 = DIRECTION ( 'NONE',  ( 0.000000000000000000, 1.000000000000000000, 0.000000000000000000 ) ) ;
#17415 = ADVANCED_FACE ( 'NONE', ( #24731 ), #10249, .F. ) ;
#17416 = ORIENTED_EDGE ( 'NONE', *, *, #27539, .F. ) ;
#17417 = CARTESIAN_POINT ( 'NONE',  ( -0.1968503937007874127, 4.336421259842520449E-17, 0.09092130223458683158 ) ) ;
#17418 = CARTESIAN_POINT ( 'NONE',  ( -0.4889536969035060410, 0.06441834428466772233, -1.550196850393700920 ) ) ;
#17419 = CARTESIAN_POINT ( 'NONE',  ( 0.2031943647053748025, 0.4121342552748526455, -1.928289503579147190 ) ) ;
#17420 = AXIS2_PLACEMENT_3D ( 'NONE', #21619, #8479, #10872 ) ;
#17421 = ADVANCED_BREP_SHAPE_REPRESENTATION ( 'O-Ring 36.5x2.65', ( #21602, #11588 ), #12073 ) ;
#17422 = APPLICATION_PROTOCOL_DEFINITION ( 'draft international standard', 'automotive_design', 1998, #25319 ) ;
#17423 = CARTESIAN_POINT ( 'NONE',  ( -0.5375739373539409893, 0.4296723508511047229, 0.3401574803149606252 ) ) ;
#17424 = CARTESIAN_POINT ( 'NONE',  ( 0.3149606299212598381, 0.000000000000000000, -3.745078740157480546 ) ) ;
#17425 = CIRCLE ( 'NONE', #18772, 0.1673228346456692994 ) ;
#17426 = ORIENTED_EDGE ( 'NONE', *, *, #5572, .F. ) ;
#17427 = DIRECTION ( 'NONE',  ( 0.6234898018587334834, 0.7818314824680296926, 0.000000000000000000 ) ) ;
#17428 = ( CONVERSION_BASED_UNIT ( 'INCH', #10652 ) LENGTH_UNIT ( ) NAMED_UNIT ( #12671 ) ) ;
#17429 = CARTESIAN_POINT ( 'NONE',  ( -0.1378076643338853602, -0.5144970376935932288, 1.747047244094488194 ) ) ;
#17430 = FACE_BOUND ( 'NONE', #2428, .T. ) ;
#17431 = DIRECTION ( 'NONE',  ( 0.000000000000000000, 0.000000000000000000, 1.000000000000000000 ) ) ;
#17432 = CARTESIAN_POINT ( 'NONE',  ( -0.6145042738822253936, -0.6192718686174618625, 0.9188498711560100229 ) ) ;
#17433 = DIRECTION ( 'NONE',  ( 1.000000000000000000, 0.000000000000000000, 0.000000000000000000 ) ) ;
#17434 = VERTEX_POINT ( 'NONE', #8080 ) ;
#17435 = DIRECTION ( 'NONE',  ( 1.000000000000000000, 0.000000000000000000, 0.000000000000000000 ) ) ;
#17436 = CARTESIAN_POINT ( 'NONE',  ( 0.000000000000000000, 0.000000000000000000, 0.1992125984251968684 ) ) ;
#17437 = CARTESIAN_POINT ( 'NONE',  ( -0.7874015748031496509, 0.3058301319751310920, -0.2956682880063846164 ) ) ;
#17438 = ORIENTED_EDGE ( 'NONE', *, *, #5227, .T. ) ;
#17439 = EDGE_CURVE ( 'NONE', #12161, #10143, #25157, .T. ) ;
#17440 = CARTESIAN_POINT ( 'NONE',  ( -0.3599896729929454864, 0.2761764805255169652, -1.934055118110236338 ) ) ;
#17441 = AXIS2_PLACEMENT_3D ( 'NONE', #12281, #8194, #14723 ) ;
#17442 = DIRECTION ( 'NONE',  ( 0.3420201433256690460, -0.9396926207859084279, 0.000000000000000000 ) ) ;
#17443 = CARTESIAN_POINT ( 'NONE',  ( 0.000000000000000000, 0.000000000000000000, 0.1771653543307086520 ) ) ;
#17444 = ORIENTED_EDGE ( 'NONE', *, *, #21977, .T. ) ;
#17445 = CARTESIAN_POINT ( 'NONE',  ( 0.5131133041954354379, -0.2529800193559368360, 0.9399606299212598381 ) ) ;
#17446 = VECTOR ( 'NONE', #8824, 39.37007874015748143 ) ;
#17447 = EDGE_CURVE ( 'NONE', #18606, #26549, #10513, .T. ) ;
#17448 = CARTESIAN_POINT ( 'NONE',  ( 0.1522836969735573143, -0.2938892803217901806, -0.3971963147566889840 ) ) ;
#17449 = DIRECTION ( 'NONE',  ( 0.000000000000000000, 0.000000000000000000, 1.000000000000000000 ) ) ;
#17450 = ADVANCED_FACE ( 'NONE', ( #1706 ), #20782, .T. ) ;
#17451 = CIRCLE ( 'NONE', #5260, 0.4921259842519685179 ) ;
#17452 = DIRECTION ( 'NONE',  ( 0.000000000000000000, 0.000000000000000000, -1.000000000000000000 ) ) ;
#17453 = CARTESIAN_POINT ( 'NONE',  ( -0.2962590301041646557, 0.2272836761397697136, -3.115157480314960647 ) ) ;
#17454 = EDGE_CURVE ( 'NONE', #1755, #23254, #14607, .T. ) ;
#17455 = CARTESIAN_POINT ( 'NONE',  ( -0.1771653543307086520, 0.000000000000000000, 0.000000000000000000 ) ) ;
#17456 = DIRECTION ( 'NONE',  ( -0.000000000000000000, -0.000000000000000000, 1.000000000000000000 ) ) ;
#17457 = CARTESIAN_POINT ( 'NONE',  ( 0.000000000000000000, 0.000000000000000000, -0.1740172276534823204 ) ) ;
#17458 = VERTEX_POINT ( 'NONE', #16836 ) ;
#17459 = CARTESIAN_POINT ( 'NONE',  ( -0.1447526197146041249, -0.3977045540727763839, 0.1377952755905511861 ) ) ;
#17460 = EDGE_CURVE ( 'NONE', #21648, #19560, #22327, .T. ) ;
#17461 = ORIENTED_EDGE ( 'NONE', *, *, #5965, .T. ) ;
#17462 = AXIS2_PLACEMENT_3D ( 'NONE', #22469, #1558, #3230 ) ;
#17463 = ORIENTED_EDGE ( 'NONE', *, *, #1399, .T. ) ;
#17464 = CARTESIAN_POINT ( 'NONE',  ( 0.3751294191746887274, 0.2999672986753446624, 0.2529987172518466387 ) ) ;
#17465 = CARTESIAN_POINT ( 'NONE',  ( 0.4792483803810960730, 0.08390985360584736485, 0.1075369453467489578 ) ) ;
#17466 = CARTESIAN_POINT ( 'NONE',  ( -0.4069448477556103505, 0.3121994997598293020, 1.766732283464566899 ) ) ;
#17467 = CARTESIAN_POINT ( 'NONE',  ( -0.4069448477556027455, 0.3121994997598392940, 1.747047244094488194 ) ) ;
#17468 = FACE_OUTER_BOUND ( 'NONE', #2550, .T. ) ;
#17469 = CIRCLE ( 'NONE', #11157, 0.4811133748141622202 ) ;
#17470 = ORIENTED_EDGE ( 'NONE', *, *, #4185, .F. ) ;
#17472 = CARTESIAN_POINT ( 'NONE',  ( 0.2962590301041578278, 0.2272836761397798999, -3.115157480314960647 ) ) ;
#17471 = CARTESIAN_POINT ( 'NONE',  ( 0.5981657849660177995, 0.4807043897637795493, 0.000000000000000000 ) ) ;
#17473 = ORIENTED_EDGE ( 'NONE', *, *, #12159, .T. ) ;
#17474 = CARTESIAN_POINT ( 'NONE',  ( -8.919671568592927398E-17, -0.7283464566929134243, 0.01181102362204724393 ) ) ;
#17475 = CARTESIAN_POINT ( 'NONE',  ( 0.1512183756282267089, 0.2841060247040496090, -0.3980637497190844809 ) ) ;
#17476 = ORIENTED_EDGE ( 'NONE', *, *, #19683, .T. ) ;
#17477 = EDGE_CURVE ( 'NONE', #17310, #24685, #23377, .T. ) ;
#17478 = CYLINDRICAL_SURFACE ( 'NONE', #10510, 0.06889763779527552368 ) ;
#17479 = EDGE_LOOP ( 'NONE', ( #13534, #5894, #6147, #4782 ) ) ;
#17480 = VERTEX_POINT ( 'NONE', #27572 ) ;
#17481 = EDGE_LOOP ( 'NONE', ( #23966, #3456, #15382, #27109, #12488 ) ) ;
#17482 = EDGE_CURVE ( 'NONE', #8860, #18722, #21642, .T. ) ;
#17484 = DIRECTION ( 'NONE',  ( -1.000000000000000000, 0.000000000000000000, 0.000000000000000000 ) ) ;
#17485 = CARTESIAN_POINT ( 'NONE',  ( 0.4333973147258542991, -0.2509079296564015737, 0.09685039370078740717 ) ) ;
#17486 = COLOUR_RGB ( '', 0.09019608, 0.27058824, 0.51372549) ;
#17487 = CARTESIAN_POINT ( 'NONE',  ( 0.6808530955049936217, 0.7992025625531264943, -0.04107133681405187448 ) ) ;
#17488 = EDGE_LOOP ( 'NONE', ( #26933, #10089, #17719, #19187 ) ) ;
#17489 = EDGE_CURVE ( 'NONE', #25766, #13641, #26964, .T. ) ;
#17490 = AXIS2_PLACEMENT_3D ( 'NONE', #4840, #1183, #17694 ) ;
#17491 = DIRECTION ( 'NONE',  ( -0.9790454724845842893, 0.2036417511401760472, 0.000000000000000000 ) ) ;
#17492 = ADVANCED_FACE ( 'NONE', ( #10171 ), #2581, .F. ) ;
#17493 = CONTEXT_DEPENDENT_SHAPE_REPRESENTATION ( #120, #26501 ) ;
#17494 = CARTESIAN_POINT ( 'NONE',  ( -0.5636180690721820374, 1.118968434182232574, 0.03326447829218234092 ) ) ;
#17495 = CYLINDRICAL_SURFACE ( 'NONE', #17786, 0.7874015748031496509 ) ;
#17496 = DIRECTION ( 'NONE',  ( -1.000000000000000000, 0.000000000000000000, 0.000000000000000000 ) ) ;
#17497 = TOROIDAL_SURFACE ( 'NONE', #22928, 0.4232283464566928832, 0.07677165354330708902 ) ;
#17498 = CIRCLE ( 'NONE', #9896, 0.5905511811023621549 ) ;
#17499 = CARTESIAN_POINT ( 'NONE',  ( -0.04956879678462303151, 0.2165354330708661457, -3.186635197791187757 ) ) ;
#17500 = EDGE_LOOP ( 'NONE', ( #2280, #21524, #8970, #17664, #5098, #10613 ) ) ;
#17501 = CIRCLE ( 'NONE', #5322, 0.3937007873768824662 ) ;
#17502 = VERTEX_POINT ( 'NONE', #27424 ) ;
#17503 = DIRECTION ( 'NONE',  ( 0.9790454724845839563, 0.1018208755700887314, 0.1763589297585421989 ) ) ;
#17504 = CARTESIAN_POINT ( 'NONE',  ( 0.2816986811832786208, -0.2161891097065020695, 1.953740157480315043 ) ) ;
#17505 = ORIENTED_EDGE ( 'NONE', *, *, #17289, .T. ) ;
#17506 = DIRECTION ( 'NONE',  ( 0.000000000000000000, 0.000000000000000000, 1.000000000000000000 ) ) ;
#17507 = EDGE_CURVE ( 'NONE', #27155, #8846, #4841, .T. ) ;
#17508 = B_SPLINE_CURVE_WITH_KNOTS ( 'NONE', 3,
 ( #1394, #10014, #27544, #9873, #7768, #24985 ),
 .UNSPECIFIED., .F., .F.,
 ( 4, 2, 4 ),
 ( 0.7157687286427130147, 0.7172350147555660582, 0.7187013008684189908 ),
 .UNSPECIFIED. ) ;
#17509 = CARTESIAN_POINT ( 'NONE',  ( -0.1634143070176771462, -0.4472844159263525965, 0.1212655228098387938 ) ) ;
#17510 = CARTESIAN_POINT ( 'NONE',  ( 0.7214243740400071436, -0.1654689342656250894, 0.2161412452787339344 ) ) ;
#17511 = DIRECTION ( 'NONE',  ( 0.000000000000000000, -1.000000000000000000, 0.000000000000000000 ) ) ;
#17512 = AXIS2_PLACEMENT_3D ( 'NONE', #26160, #19672, #6537 ) ;
#17513 = ORIENTED_EDGE ( 'NONE', *, *, #12405, .F. ) ;
#17514 = CARTESIAN_POINT ( 'NONE',  ( 0.4954197419817713000, 0.2442565704126274662, 0.9399606299212598381 ) ) ;
#17515 = VERTEX_POINT ( 'NONE', #9033 ) ;
#17516 = EDGE_CURVE ( 'NONE', #5769, #22371, #25171, .T. ) ;
#17517 = CARTESIAN_POINT ( 'NONE',  ( -0.6562077975700374433, -1.365924015748031427E-17, -0.2362204724409449064 ) ) ;
#17518 = ORIENTED_EDGE ( 'NONE', *, *, #16818, .F. ) ;
#17519 = DIRECTION ( 'NONE',  ( 0.000000000000000000, 0.000000000000000000, 1.000000000000000000 ) ) ;
#17520 = CARTESIAN_POINT ( 'NONE',  ( 0.6614173228346456046, 8.100026073100603114E-17, -0.1309055118110236116 ) ) ;
#17521 = CARTESIAN_POINT ( 'NONE',  ( 9.642888182478974314E-17, 0.1968503937007874127, 0.7874015748208159637 ) ) ;
#17522 = CIRCLE ( 'NONE', #5337, 0.1299232283464567539 ) ;
#17523 = CARTESIAN_POINT ( 'NONE',  ( 0.000000000000000000, 0.000000000000000000, 0.3543307086614173040 ) ) ;
#17524 = CIRCLE ( 'NONE', #13005, 0.2395669291338582696 ) ;
#17525 = CARTESIAN_POINT ( 'NONE',  ( -0.3874223757830720927, 0.3097832252370624206, 0.2989974301407470891 ) ) ;
#17526 = DIRECTION ( 'NONE',  ( 0.000000000000000000, 1.000000000000000000, 0.000000000000000000 ) ) ;
#17527 = ORIENTED_EDGE ( 'NONE', *, *, #16341, .T. ) ;
#17528 = STYLED_ITEM ( 'NONE', ( #6149 ), #3396 ) ;
#17529 = DIRECTION ( 'NONE',  ( 0.000000000000000000, -1.000000000000000000, 0.000000000000000000 ) ) ;
#17530 = EDGE_CURVE ( 'NONE', #23783, #17886, #9833, .T. ) ;
#17531 = VERTEX_POINT ( 'NONE', #15558 ) ;
#17532 = CARTESIAN_POINT ( 'NONE',  ( -0.5905511811023621549, 0.000000000000000000, 0.000000000000000000 ) ) ;
#17533 = CARTESIAN_POINT ( 'NONE',  ( 0.000000000000000000, 0.4724409448818898127, 0.000000000000000000 ) ) ;
#17534 = CARTESIAN_POINT ( 'NONE',  ( 0.1839420097223146422, 0.5417097841049177687, 0.9399606299212598381 ) ) ;
#17535 = CONICAL_SURFACE ( 'NONE', #13034, 2.066929133858267598, 0.7853981624999996081 ) ;
#17536 = CARTESIAN_POINT ( 'NONE',  ( 0.000000000000000000, 0.000000000000000000, 0.2362204724409449064 ) ) ;
#17537 = VERTEX_POINT ( 'NONE', #19365 ) ;
#17538 = CARTESIAN_POINT ( 'NONE',  ( -0.4684132450478833976, -0.1062614382955279213, 0.2529987172372142878 ) ) ;
#17539 = B_SPLINE_CURVE_WITH_KNOTS ( 'NONE', 3,
 ( #9764, #27430, #3386, #8083, #14599, #16697 ),
 .UNSPECIFIED., .F., .F.,
 ( 4, 2, 4 ),
 ( 0.5000000000000000000, 0.7500000000000000000, 1.000000000000000000 ),
 .UNSPECIFIED. ) ;
#17540 = ORIENTED_EDGE ( 'NONE', *, *, #21194, .F. ) ;
#17541 = CIRCLE ( 'NONE', #15335, 0.3464566929133857665 ) ;
#17542 = ORIENTED_EDGE ( 'NONE', *, *, #23370, .F. ) ;
#17543 = CIRCLE ( 'NONE', #13454, 0.6299212598425196763 ) ;
#17544 = DIRECTION ( 'NONE',  ( -0.9790454724845842893, -0.2036417511401760472, 2.493892000000000781E-17 ) ) ;
#17545 = CARTESIAN_POINT ( 'NONE',  ( 0.3135473077061334268, 3.839847067635865072E-17, 2.504921259842519898 ) ) ;
#17546 = VECTOR ( 'NONE', #26040, 39.37007874015748143 ) ;
#17547 = FACE_BOUND ( 'NONE', #11595, .T. ) ;
#17548 = CARTESIAN_POINT ( 'NONE',  ( 0.3606049308168208234, 0.06410376196655420689, 0.08455817587496759768 ) ) ;
#17549 = EDGE_LOOP ( 'NONE', ( #4141, #7750 ) ) ;
#17550 = EDGE_CURVE ( 'NONE', #4548, #22985, #3505, .T. ) ;
#17551 = CARTESIAN_POINT ( 'NONE',  ( 0.000000000000000000, 0.000000000000000000, 0.1771653543307086520 ) ) ;
#17552 = ORIENTED_EDGE ( 'NONE', *, *, #4591, .F. ) ;
#17553 = ORIENTED_EDGE ( 'NONE', *, *, #5688, .T. ) ;
#17554 = CARTESIAN_POINT ( 'NONE',  ( 0.5190862322091315262, -0.1177929122753177127, 0.3401574803149606252 ) ) ;
#17555 = CONICAL_SURFACE ( 'NONE', #24299, 1.112204724409448842, 0.7853981625000011624 ) ;
#17556 = CARTESIAN_POINT ( 'NONE',  ( 5.827097576719993621E-17, 0.6881889763779529545, 0.3401599409343964431 ) ) ;
#17557 = LINE ( 'NONE', #21384, #9093 ) ;
#17558 = CARTESIAN_POINT ( 'NONE',  ( -0.3268939675028499914, -0.1881330340946393564, 0.1992125984251968684 ) ) ;
#17559 = CARTESIAN_POINT ( 'NONE',  ( -0.3334645669291338987, 5.862181872992126152E-06, -1.869015748010449007 ) ) ;
#17560 = DIRECTION ( 'NONE',  ( 0.000000000000000000, 0.000000000000000000, 1.000000000000000000 ) ) ;
#17561 = EDGE_CURVE ( 'NONE', #21486, #20876, #19317, .T. ) ;
#17562 = ORIENTED_EDGE ( 'NONE', *, *, #23316, .F. ) ;
#17563 = DIRECTION ( 'NONE',  ( -0.9575713608335526539, -0.1440981340193016325, -0.2495852893972989595 ) ) ;
#17564 = CARTESIAN_POINT ( 'NONE',  ( 1.244982677165354375E-18, -0.09092130223458683158, -0.4724409448818898127 ) ) ;
#17565 = CARTESIAN_POINT ( 'NONE',  ( -0.4270824798167697223, -0.2466292688015108703, -1.569881889763779625 ) ) ;
#17566 = AXIS2_PLACEMENT_3D ( 'NONE', #26665, #20881, #975 ) ;
#17567 = CARTESIAN_POINT ( 'NONE',  ( 0.3979194638820598984, -0.2297883689023126064, -1.928289503579157183 ) ) ;
#17568 = CARTESIAN_POINT ( 'NONE',  ( 0.3454440660767517657, -0.3030032861724969440, -1.928289503579156516 ) ) ;
#17569 = CIRCLE ( 'NONE', #26554, 0.01377952755905510404 ) ;
#17570 = CARTESIAN_POINT ( 'NONE',  ( -0.2762247810519002922, 0.4783323773986519201, 0.9202755905511811330 ) ) ;
#17571 = VECTOR ( 'NONE', #19685, 39.37007874015748854 ) ;
#17572 = CARTESIAN_POINT ( 'NONE',  ( 0.09842519685039370636, 0.2991866959364303247, -3.548228346456693050 ) ) ;
#17573 = CARTESIAN_POINT ( 'NONE',  ( -0.0006812437162517212324, 0.6577569867587390595, 0.2081850588307845862 ) ) ;
#17574 = EDGE_CURVE ( 'NONE', #18836, #13154, #18921, .T. ) ;
#17575 = CARTESIAN_POINT ( 'NONE',  ( 0.1287090038540880110, 0.1704774416898509615, -0.09842519685039369248 ) ) ;
#17576 = ORIENTED_EDGE ( 'NONE', *, *, #24370, .F. ) ;
#17577 = DIRECTION ( 'NONE',  ( 0.000000000000000000, 0.000000000000000000, 1.000000000000000000 ) ) ;
#17578 = CARTESIAN_POINT ( 'NONE',  ( 0.6202606299212598540, 0.08876456692913387014, 1.087052427674648014E-17 ) ) ;
#17579 = CARTESIAN_POINT ( 'NONE',  ( -0.6633461167951516524, 0.01962289458785622040, -0.07887503487148522785 ) ) ;
#17580 = ORIENTED_EDGE ( 'NONE', *, *, #20606, .F. ) ;
#17581 = ORIENTED_EDGE ( 'NONE', *, *, #25869, .F. ) ;
#17582 = CARTESIAN_POINT ( 'NONE',  ( 0.5118110236220472231, 3.133938659235352953E-17, 1.766732283464566899 ) ) ;
#17583 = AXIS2_PLACEMENT_3D ( 'NONE', #18298, #5324, #9543 ) ;
#17584 = DIRECTION ( 'NONE',  ( -0.9396926207859083169, 0.3420201433256692125, 0.000000000000000000 ) ) ;
#17585 = CARTESIAN_POINT ( 'NONE',  ( 0.000000000000000000, 0.3771653543307086909, 0.03818897637795275884 ) ) ;
#17586 = FACE_OUTER_BOUND ( 'NONE', #19216, .T. ) ;
#17587 = CARTESIAN_POINT ( 'NONE',  ( 0.02438677169350789847, 0.3726024258163779246, -3.115157480314960647 ) ) ;
#17588 = CARTESIAN_POINT ( 'NONE',  ( 0.000000000000000000, 0.000000000000000000, 0.1377952755905511584 ) ) ;
#17589 = DIRECTION ( 'NONE',  ( 0.000000000000000000, 0.000000000000000000, 1.000000000000000000 ) ) ;
#17590 = VERTEX_POINT ( 'NONE', #24157 ) ;
#17591 = CARTESIAN_POINT ( 'NONE',  ( 0.1288129352161812846, -0.4793172621399190425, -1.569881889763779403 ) ) ;
#17592 = EDGE_CURVE ( 'NONE', #9997, #25216, #25630, .T. ) ;
#17593 = CIRCLE ( 'NONE', #4083, 0.3937007874015748254 ) ;
#17594 = CIRCLE ( 'NONE', #4965, 0.6212598425196850238 ) ;
#17595 = ORIENTED_EDGE ( 'NONE', *, *, #13073, .F. ) ;
#17596 = VERTEX_POINT ( 'NONE', #13409 ) ;
#17597 = DIRECTION ( 'NONE',  ( 0.7660444431189777914, -0.6427876096865396960, 0.000000000000000000 ) ) ;
#17598 = DIRECTION ( 'NONE',  ( 0.000000000000000000, 0.000000000000000000, 1.000000000000000000 ) ) ;
#17599 = DIRECTION ( 'NONE',  ( -1.000000000000000000, 0.000000000000000000, 0.000000000000000000 ) ) ;
#17600 = ADVANCED_FACE ( 'NONE', ( #22036 ), #26270, .T. ) ;
#17601 = FACE_OUTER_BOUND ( 'NONE', #27680, .T. ) ;
#17602 = VERTEX_POINT ( 'NONE', #15426 ) ;
#17603 = VECTOR ( 'NONE', #3848, 39.37007874015748143 ) ;
#17604 = ORIENTED_EDGE ( 'NONE', *, *, #24323, .F. ) ;
#17606 = CARTESIAN_POINT ( 'NONE',  ( 0.04877294052295595012, 0.3702005978258479102, -3.115157480314960647 ) ) ;
#17605 = CARTESIAN_POINT ( 'NONE',  ( 0.5385210225480960844, 0.4284847435812472183, 0.1322834645669291320 ) ) ;
#17607 = ADVANCED_FACE ( 'NONE', ( #21490 ), #24017, .T. ) ;
#17608 = ORIENTED_EDGE ( 'NONE', *, *, #8946, .F. ) ;
#17609 = FACE_BOUND ( 'NONE', #6840, .T. ) ;
#17610 = DIRECTION ( 'NONE',  ( 0.000000000000000000, 0.000000000000000000, -1.000000000000000000 ) ) ;
#17611 = ORIENTED_EDGE ( 'NONE', *, *, #25900, .F. ) ;
#17612 = CARTESIAN_POINT ( 'NONE',  ( 0.08676778863011140597, -0.3239425792934415571, 1.953740157480315043 ) ) ;
#17613 = EDGE_LOOP ( 'NONE', ( #13756, #27661, #21505, #1092, #16338, #25006, #25856 ) ) ;
#17614 = VERTEX_POINT ( 'NONE', #8626 ) ;
#17615 = CARTESIAN_POINT ( 'NONE',  ( 0.3263749705684267921, -0.1890319631540330891, 0.1992125984251968684 ) ) ;
#17616 = FACE_OUTER_BOUND ( 'NONE', #5904, .T. ) ;
#17617 = EDGE_LOOP ( 'NONE', ( #25888, #9529, #6974, #24977 ) ) ;
#17618 = VERTEX_POINT ( 'NONE', #10747 ) ;
#17619 = ORIENTED_EDGE ( 'NONE', *, *, #11814, .T. ) ;
#17620 = CARTESIAN_POINT ( 'NONE',  ( -0.1918813796216842782, -0.5271897577243779276, 0.1771653543307086520 ) ) ;
#17621 = AXIS2_PLACEMENT_3D ( 'NONE', #22987, #5754, #23271 ) ;
#17622 = CARTESIAN_POINT ( 'NONE',  ( 0.3765118517642104257, -2.263258471485603576E-17, -3.100567304031763172 ) ) ;
#17623 = CARTESIAN_POINT ( 'NONE',  ( 0.09590060490395689585, -0.1136516277932324709, -0.1968503937007874127 ) ) ;
#17624 = CARTESIAN_POINT ( 'NONE',  ( 0.7434810862212987148, 0.6612525179033372780, 0.05419551519301178677 ) ) ;
#17625 = ORIENTED_EDGE ( 'NONE', *, *, #21838, .F. ) ;
#17626 = FACE_OUTER_BOUND ( 'NONE', #13031, .T. ) ;
#17627 = CARTESIAN_POINT ( 'NONE',  ( -0.03532354024591893848, -0.8267716535433070613, 0.7500000000000001110 ) ) ;
#17628 = EDGE_CURVE ( 'NONE', #14152, #20711, #23985, .T. ) ;
#17629 = CARTESIAN_POINT ( 'NONE',  ( -0.01935208613492874971, -0.07974837009520491238, -0.4684893292439904489 ) ) ;
#17630 = CARTESIAN_POINT ( 'NONE',  ( 0.07874015748031495954, 0.01168837908608117392, -0.4660229470383086547 ) ) ;
#17631 = CARTESIAN_POINT ( 'NONE',  ( -0.03532354024591901481, -0.8267716535433071723, 0.000000000000000000 ) ) ;
#17632 = ADVANCED_FACE ( 'NONE', ( #11025 ), #8492, .F. ) ;
#17633 = CIRCLE ( 'NONE', #15409, 0.1181102362204720091 ) ;
#17634 = DIRECTION ( 'NONE',  ( -0.000000000000000000, -0.000000000000000000, -1.000000000000000000 ) ) ;
#17635 = VERTEX_POINT ( 'NONE', #21630 ) ;
#17636 = PLANE ( 'NONE',  #18932 ) ;
#17637 = LENGTH_MEASURE_WITH_UNIT ( LENGTH_MEASURE( 0.02539999999999999897 ), #24002 ) ;
#17638 = ORIENTED_EDGE ( 'NONE', *, *, #16708, .T. ) ;
#17639 = DIRECTION ( 'NONE',  ( -1.000000000000000000, 0.000000000000000000, 0.000000000000000000 ) ) ;
#17640 = AXIS2_PLACEMENT_3D ( 'NONE', #24284, #22034, #4930 ) ;
#17641 = FACE_OUTER_BOUND ( 'NONE', #6758, .T. ) ;
#17642 = CARTESIAN_POINT ( 'NONE',  ( 0.09842519685039370636, 0.5905905511811023745, -3.548228346456693050 ) ) ;
#17643 = B_SPLINE_CURVE_WITH_KNOTS ( 'NONE', 3,
 ( #621, #2986, #9343, #2847, #11485, #17954, #22363, #26588, #9488, #18085 ),
 .UNSPECIFIED., .F., .F.,
 ( 4, 2, 2, 2, 4 ),
 ( 0.000000000000000000, 0.2500000000000000000, 0.5000000000000000000, 0.7500000000000000000, 1.000000000000000000 ),
 .UNSPECIFIED. ) ;
#17644 = ORIENTED_EDGE ( 'NONE', *, *, #24503, .F. ) ;
#17645 = CARTESIAN_POINT ( 'NONE',  ( 0.3362148458988353239, 0.4382482975805538361, 0.9399606299212598381 ) ) ;
#17646 = ORIENTED_EDGE ( 'NONE', *, *, #17751, .F. ) ;
#17647 = CARTESIAN_POINT ( 'NONE',  ( 0.000000000000000000, 0.5610236220472440971, 0.3543307086614173040 ) ) ;
#17648 = EDGE_CURVE ( 'NONE', #4007, #15131, #1271, .T. ) ;
#17649 = CARTESIAN_POINT ( 'NONE',  ( 0.1694923354742838562, -0.4674199084401557402, 0.1615162260937435257 ) ) ;
#17650 = CARTESIAN_POINT ( 'NONE',  ( -0.1968503937007874127, -5.802129921259842692E-18, 0.000000000000000000 ) ) ;
#17651 = LINE ( 'NONE', #6937, #8688 ) ;
#17652 = FACE_OUTER_BOUND ( 'NONE', #3148, .T. ) ;
#17653 = CIRCLE ( 'NONE', #9996, 0.4692913385826771866 ) ;
#17654 = CARTESIAN_POINT ( 'NONE',  ( -0.4055118110236220486, -0.4724409448818898127, 0.8182917201112794858 ) ) ;
#17655 = CARTESIAN_POINT ( 'NONE',  ( -0.5314960629921260393, 6.402768735150616610E-17, 1.747047244094488194 ) ) ;
#17656 = ADVANCED_FACE ( 'NONE', ( #26002 ), #11642, .T. ) ;
#17657 = B_SPLINE_CURVE_WITH_KNOTS ( 'NONE', 3,
 ( #12105, #27517, #27229, #1932, #1651, #19158, #10540, #21007, #21148, #18737, #25243, #4059, #14819, #19021, #10257, #25100, #22852, #8025, #25382, #5905, #12665, #27796, #20728, #25668, #1373, #9987, #18585, #14679, #23136, #27655, #22997, #7879, #8432, #1512 ),
 .UNSPECIFIED., .F., .F.,
 ( 4, 2, 2, 2, 2, 2, 2, 2, 2, 2, 2, 2, 2, 2, 2, 2, 4 ),
 ( 0.5000000000000000000, 0.5312500000000000000, 0.5625000000000000000, 0.5937500000000000000, 0.6250000000000000000, 0.6562500000000000000, 0.6875000000000000000, 0.7187500000000000000, 0.7500000000000000000, 0.7812500000000000000, 0.8125000000000000000, 0.8437500000000000000, 0.8750000000000000000, 0.9062500000000000000, 0.9375000000000000000, 0.9687500000000000000, 1.000000000000000000 ),
 .UNSPECIFIED. ) ;
#17658 = CARTESIAN_POINT ( 'NONE',  ( -0.5671862884095228985, -0.07472527936312044206, 0.9399606299212598381 ) ) ;
#17659 = CARTESIAN_POINT ( 'NONE',  ( 0.4092783051644229841, -0.3145317858139328737, 1.766732283464567121 ) ) ;
#17660 = ORIENTED_EDGE ( 'NONE', *, *, #9364, .F. ) ;
#17661 = DIRECTION ( 'NONE',  ( 0.000000000000000000, 0.000000000000000000, 1.000000000000000000 ) ) ;
#17662 = CARTESIAN_POINT ( 'NONE',  ( -0.6299212598425196763, -0.4526313213353582721, -0.9943460912301771426 ) ) ;
#17663 = ADVANCED_FACE ( 'NONE', ( #446, #322 ), #24556, .T. ) ;
#17664 = ORIENTED_EDGE ( 'NONE', *, *, #10960, .F. ) ;
#17665 = EDGE_CURVE ( 'NONE', #10762, #21585, #8925, .T. ) ;
#17666 = ORIENTED_EDGE ( 'NONE', *, *, #25563, .F. ) ;
#17667 = AXIS2_PLACEMENT_3D ( 'NONE', #2262, #4256, #8898 ) ;
#17668 = CYLINDRICAL_SURFACE ( 'NONE', #27331, 0.3937007874015748254 ) ;
#17669 = DIRECTION ( 'NONE',  ( 0.000000000000000000, 0.000000000000000000, -1.000000000000000000 ) ) ;
#17670 = FACE_BOUND ( 'NONE', #24653, .T. ) ;
#17671 = DIRECTION ( 'NONE',  ( 0.000000000000000000, 1.000000000000000000, 0.000000000000000000 ) ) ;
#17672 = DIRECTION ( 'NONE',  ( 0.000000000000000000, 0.000000000000000000, -1.000000000000000000 ) ) ;
#17673 = EDGE_LOOP ( 'NONE', ( #4672, #12209, #4960, #4076 ) ) ;
#17674 = ( GEOMETRIC_REPRESENTATION_CONTEXT ( 3 ) GLOBAL_UNCERTAINTY_ASSIGNED_CONTEXT ( ( #22888 ) ) GLOBAL_UNIT_ASSIGNED_CONTEXT ( ( #17428, #23937, #8813 ) ) REPRESENTATION_CONTEXT ( 'NONE', 'WORKASPACE' ) ) ;
#17675 = FACE_OUTER_BOUND ( 'NONE', #4423, .T. ) ;
#17676 = CARTESIAN_POINT ( 'NONE',  ( -0.3149606299212598381, 0.000000000000000000, 0.000000000000000000 ) ) ;
#17677 = CARTESIAN_POINT ( 'NONE',  ( 0.4895462770358314786, 0.7878044190917184997, -0.4800777499788905778 ) ) ;
#17678 = ORIENTED_EDGE ( 'NONE', *, *, #10852, .T. ) ;
#17679 = FACE_OUTER_BOUND ( 'NONE', #5478, .T. ) ;
#17680 = ORIENTED_EDGE ( 'NONE', *, *, #18332, .F. ) ;
#17681 = CARTESIAN_POINT ( 'NONE',  ( 0.4130706566799093316, -0.3346769814300175616, -0.5796775359605755851 ) ) ;
#17682 = CARTESIAN_POINT ( 'NONE',  ( 0.4232283464566928832, 0.000000000000000000, 0.1377952755905511861 ) ) ;
#17683 = CARTESIAN_POINT ( 'NONE',  ( -0.3121994997578197428, 0.4069448477569481692, -1.550196850393700920 ) ) ;
#17684 = CARTESIAN_POINT ( 'NONE',  ( 0.4121342552748534227, 0.2031943647053804092, -1.928289503579144304 ) ) ;
#17685 = EDGE_LOOP ( 'NONE', ( #1900, #4577 ) ) ;
#17686 = EDGE_CURVE ( 'NONE', #22611, #12126, #24265, .T. ) ;
#17687 = CARTESIAN_POINT ( 'NONE',  ( -0.4954197419817560344, 0.2442565704126489212, 0.9202755905511811330 ) ) ;
#17688 = CARTESIAN_POINT ( 'NONE',  ( 0.3218517393630221934, 0.3826375019112421283, 0.1496602734594676132 ) ) ;
#17689 = EDGE_CURVE ( 'NONE', #12475, #14000, #26072, .T. ) ;
#17690 = DIRECTION ( 'NONE',  ( 0.000000000000000000, 1.000000000000000000, 0.000000000000000000 ) ) ;
#17691 = EDGE_CURVE ( 'NONE', #24515, #23576, #12094, .T. ) ;
#17692 = DIRECTION ( 'NONE',  ( 0.000000000000000000, 0.000000000000000000, 1.000000000000000000 ) ) ;
#17693 = CARTESIAN_POINT ( 'NONE',  ( 2.632951206231566310, -0.4724409448818898127, -0.9491381768041949885 ) ) ;
#17694 = DIRECTION ( 'NONE',  ( 0.000000000000000000, -1.000000000000000000, 0.000000000000000000 ) ) ;
#17695 = FACE_OUTER_BOUND ( 'NONE', #15350, .T. ) ;
#17696 = EDGE_CURVE ( 'NONE', #13891, #6621, #22728, .T. ) ;
#17697 = CARTESIAN_POINT ( 'NONE',  ( -0.6050288667202972093, -0.5969381639782070925, 0.9446416071478749288 ) ) ;
#17698 = CARTESIAN_POINT ( 'NONE',  ( -0.1658556822967069411, -0.4573967274743634404, 0.2467937633334012226 ) ) ;
#17699 = VERTEX_POINT ( 'NONE', #20473 ) ;
#17700 = PRODUCT_DEFINITION_SHAPE ( 'NONE', 'NONE',  #27921 ) ;
#17701 = LINE ( 'NONE', #7245, #20416 ) ;
#17702 = CARTESIAN_POINT ( 'NONE',  ( 0.4626586504047134341, 5.665934353159666004E-17, -0.2204724409448818867 ) ) ;
#17703 = AXIS2_PLACEMENT_3D ( 'NONE', #20104, #26326, #626 ) ;
#17704 = CARTESIAN_POINT ( 'NONE',  ( 0.000000000000000000, 0.000000000000000000, 0.000000000000000000 ) ) ;
#17705 = EDGE_LOOP ( 'NONE', ( #22716, #10947, #19048, #8779 ) ) ;
#17706 = AXIS2_PLACEMENT_3D ( 'NONE', #15882, #3427, #7260 ) ;
#17707 = LINE ( 'NONE', #26331, #25664 ) ;
#17708 = DIRECTION ( 'NONE',  ( -0.000000000000000000, 1.000000000000000000, -0.000000000000000000 ) ) ;
#17709 = DIRECTION ( 'NONE',  ( 0.000000000000000000, 0.000000000000000000, -1.000000000000000000 ) ) ;
#17710 = EDGE_LOOP ( 'NONE', ( #19378, #12441, #19929, #17243 ) ) ;
#17711 = EDGE_CURVE ( 'NONE', #15797, #290, #7463, .T. ) ;
#17712 = AXIS2_PLACEMENT_3D ( 'NONE', #17121, #3840, #25454 ) ;
#17713 = CARTESIAN_POINT ( 'NONE',  ( 0.4446035140077002623, -0.02917857698668054056, -1.934055118110235894 ) ) ;
#17714 = CARTESIAN_POINT ( 'NONE',  ( -0.3644697409450256553, 0.09762295995070000010, -3.100567304031767168 ) ) ;
#17715 = DIRECTION ( 'NONE',  ( 0.000000000000000000, 1.000000000000000000, 0.000000000000000000 ) ) ;
#17716 = DIRECTION ( 'NONE',  ( 1.000000000000000000, 7.017815000000000124E-18, 0.000000000000000000 ) ) ;
#17717 = CARTESIAN_POINT ( 'NONE',  ( 0.6476458834291769495, 0.1148891961919920740, 0.1461456498338012666 ) ) ;
#17718 = APPLICATION_CONTEXT ( 'automotive_design' ) ;
#17719 = ORIENTED_EDGE ( 'NONE', *, *, #17744, .T. ) ;
#17720 = DIRECTION ( 'NONE',  ( 1.000000000000000000, 0.000000000000000000, 0.000000000000000000 ) ) ;
#17721 = AXIS2_PLACEMENT_3D ( 'NONE', #24936, #9392, #7427 ) ;
#17722 = AXIS2_PLACEMENT_3D ( 'NONE', #11191, #473, #15327 ) ;
#17723 = VERTEX_POINT ( 'NONE', #13547 ) ;
#17724 = VERTEX_POINT ( 'NONE', #16243 ) ;
#17725 = CARTESIAN_POINT ( 'NONE',  ( 0.5099673189337476931, -0.1157175986333582596, 0.3331434174568621565 ) ) ;
#17726 = VECTOR ( 'NONE', #5194, 39.37007874015748854 ) ;
#17727 = CARTESIAN_POINT ( 'NONE',  ( 0.000000000000000000, 0.000000000000000000, -4.330708661417323135 ) ) ;
#17728 = CARTESIAN_POINT ( 'NONE',  ( -0.1327036767659760530, 0.4954415918530867269, 1.747047244094488194 ) ) ;
#17729 = CARTESIAN_POINT ( 'NONE',  ( -0.6889763779527560139, 0.000000000000000000, -0.1377952755905511861 ) ) ;
#17730 = VERTEX_POINT ( 'NONE', #17903 ) ;
#17731 = AXIS2_PLACEMENT_3D ( 'NONE', #1272, #15966, #9587 ) ;
#17732 = CARTESIAN_POINT ( 'NONE',  ( 0.02438677169350789847, 0.3726024258163779246, -3.115157480314960647 ) ) ;
#17733 = VECTOR ( 'NONE', #11132, 39.37007874015748143 ) ;
#17734 = ORIENTED_EDGE ( 'NONE', *, *, #23952, .F. ) ;
#17735 = DIRECTION ( 'NONE',  ( 0.000000000000000000, 0.000000000000000000, -1.000000000000000000 ) ) ;
#17736 = CARTESIAN_POINT ( 'NONE',  ( -0.1078280746903979848, 0.3175540113612246862, 1.953740157480315043 ) ) ;
#17737 = EDGE_LOOP ( 'NONE', ( #3790, #1856, #13746, #22001 ) ) ;
#17738 = ORIENTED_EDGE ( 'NONE', *, *, #13111, .T. ) ;
#17739 = ORIENTED_EDGE ( 'NONE', *, *, #24056, .F. ) ;
#17740 = CARTESIAN_POINT ( 'NONE',  ( 0.000000000000000000, 0.09092130223458683158, -0.4724409448818898127 ) ) ;
#17741 = ORIENTED_EDGE ( 'NONE', *, *, #23315, .F. ) ;
#17742 = ORIENTED_EDGE ( 'NONE', *, *, #4465, .T. ) ;
#17743 = ORIENTED_EDGE ( 'NONE', *, *, #17751, .T. ) ;
#17744 = EDGE_CURVE ( 'NONE', #22551, #13827, #7336, .T. ) ;
#17745 = CARTESIAN_POINT ( 'NONE',  ( -0.07874015748031511219, 0.1968503937007874127, -3.558551041376953883 ) ) ;
#17746 = CLOSED_SHELL ( 'NONE', ( #10682, #20122, #9127, #15373, #3803, #18519, #4835, #5738, #5586, #5357, #8683, #9228, #13507, #20900, #21252, #15413, #9195, #3573, #2381, #13718, #20286, #24044, #9332, #14952, #22863, #19966, #12241, #9847, #12343, #1215, #9167, #12468, #1407, #18809, #14495, #22858, #8150, #15020, #11478, #15402, #6340, #23374, #11531, #10319 ) ) ;
#17747 = CARTESIAN_POINT ( 'NONE',  ( 0.2083728861314909642, 0.5236634780160394076, -0.008584350130356221617 ) ) ;
#17748 = CARTESIAN_POINT ( 'NONE',  ( -0.3183792087434620388, -0.6629319518604491757, 0.2763636194374882171 ) ) ;
#17749 = CARTESIAN_POINT ( 'NONE',  ( 0.7205383896161363655, 0.7193007239719539925, 0.01696726750475779227 ) ) ;
#17750 = ORIENTED_EDGE ( 'NONE', *, *, #23162, .F. ) ;
#17751 = EDGE_CURVE ( 'NONE', #22705, #4526, #14374, .T. ) ;
#17752 = AXIS2_PLACEMENT_3D ( 'NONE', #10436, #10022, #23602 ) ;
#17753 = DIRECTION ( 'NONE',  ( 0.000000000000000000, -1.000000000000000000, 0.000000000000000000 ) ) ;
#17754 = CYLINDRICAL_SURFACE ( 'NONE', #9179, 0.5118110236220472231 ) ;
#17755 = EDGE_CURVE ( 'NONE', #17779, #27463, #1408, .T. ) ;
#17756 = ADVANCED_FACE ( 'NONE', ( #22171 ), #17497, .F. ) ;
#17757 = AXIS2_PLACEMENT_3D ( 'NONE', #20946, #16862, #20805 ) ;
#17758 = CARTESIAN_POINT ( 'NONE',  ( -0.3543307086614173596, 0.02319089060378165187, 1.953740157480315043 ) ) ;
#17759 = FACE_OUTER_BOUND ( 'NONE', #18696, .T. ) ;
#17760 = CARTESIAN_POINT ( 'NONE',  ( -0.5905511811023621549, -0.4724409448818898127, -0.8182917201112815953 ) ) ;
#17761 = FACE_OUTER_BOUND ( 'NONE', #16139, .T. ) ;
#17762 = DIRECTION ( 'NONE',  ( -1.000000000000000000, 0.000000000000000000, 0.000000000000000000 ) ) ;
#17763 = DIRECTION ( 'NONE',  ( -0.9749279121818236193, -0.2225209339563142819, 0.000000000000000000 ) ) ;
#17764 = CIRCLE ( 'NONE', #2425, 0.09842519685039370636 ) ;
#17765 = DIRECTION ( 'NONE',  ( 0.000000000000000000, 0.000000000000000000, 1.000000000000000000 ) ) ;
#17766 = ORIENTED_EDGE ( 'NONE', *, *, #13201, .T. ) ;
#17767 = DIRECTION ( 'NONE',  ( -0.9790454724845842893, 0.1018208755700880375, 0.1763589297585410332 ) ) ;
#17768 = ( LENGTH_UNIT ( ) NAMED_UNIT ( * ) SI_UNIT ( $, .METRE. ) ) ;
#17769 = EDGE_LOOP ( 'NONE', ( #22791, #25944, #5021, #15777 ) ) ;
#17770 = CARTESIAN_POINT ( 'NONE',  ( 0.006151574803149606648, 0.000000000000000000, -0.1074461786882927178 ) ) ;
#17771 = ORIENTED_EDGE ( 'NONE', *, *, #9457, .T. ) ;
#17772 = AXIS2_PLACEMENT_3D ( 'NONE', #22636, #7810, #7378 ) ;
#17773 = LINE ( 'NONE', #10871, #25586 ) ;
#17774 = CARTESIAN_POINT ( 'NONE',  ( -0.07874015748031495954, 0.04546065111729338803, -0.3779527559055118058 ) ) ;
#17775 = EDGE_LOOP ( 'NONE', ( #15965, #20350, #10608, #26165, #3732, #21865 ) ) ;
#17776 = CARTESIAN_POINT ( 'NONE',  ( 0.5375739373539409893, 0.4296723508511047229, 0.3401574803149606252 ) ) ;
#17777 = CARTESIAN_POINT ( 'NONE',  ( 0.07214854559195596484, 0.5476281405333121022, 0.9399606299212598381 ) ) ;
#17778 = CARTESIAN_POINT ( 'NONE',  ( 0.5869493968219645641, -0.2133897621573078718, -0.3696019098714952711 ) ) ;
#17779 = VERTEX_POINT ( 'NONE', #2797 ) ;
#17780 = EDGE_CURVE ( 'NONE', #12969, #23446, #4441, .T. ) ;
#17781 = DIRECTION ( 'NONE',  ( 0.000000000000000000, 1.000000000000000000, 0.000000000000000000 ) ) ;
#17782 = DIRECTION ( 'NONE',  ( 0.000000000000000000, 0.8660254037844385966, -0.4999999999999998335 ) ) ;
#17783 = DIRECTION ( 'NONE',  ( 0.000000000000000000, 1.000000000000000000, 0.000000000000000000 ) ) ;
#17784 = CARTESIAN_POINT ( 'NONE',  ( 0.000000000000000000, 0.000000000000000000, -0.1756889763779527769 ) ) ;
#17785 = EDGE_CURVE ( 'NONE', #20978, #23007, #7624, .T. ) ;
#17786 = AXIS2_PLACEMENT_3D ( 'NONE', #23996, #9271, #7041 ) ;
#17787 = CARTESIAN_POINT ( 'NONE',  ( 0.5018154743078061530, -0.1152098006148895432, 0.3251195115541528069 ) ) ;
#17788 = EDGE_CURVE ( 'NONE', #13676, #14586, #13431, .T. ) ;
#17789 = CARTESIAN_POINT ( 'NONE',  ( 0.1677079028045289355, -0.2904160862623609840, 1.953740157480315043 ) ) ;
#17790 = DIRECTION ( 'NONE',  ( 0.000000000000000000, -1.000000000000000000, 0.000000000000000000 ) ) ;
#17791 = B_SPLINE_CURVE_WITH_KNOTS ( 'NONE', 3,
 ( #16647, #23152, #18888, #27387, #25257, #21021 ),
 .UNSPECIFIED., .F., .F.,
 ( 4, 2, 4 ),
 ( 0.5000000000000000000, 0.7500000000000000000, 1.000000000000000000 ),
 .UNSPECIFIED. ) ;
#17792 = CARTESIAN_POINT ( 'NONE',  ( 0.000000000000000000, -5.394653543307086438E-17, -0.1627508102905848297 ) ) ;
#17793 = CARTESIAN_POINT ( 'NONE',  ( 0.3992017438595160117, -0.2298214351608009742, 0.1639447408809755480 ) ) ;
#17794 = AXIS2_PLACEMENT_3D ( 'NONE', #14527, #23130, #1925 ) ;
#17795 = CARTESIAN_POINT ( 'NONE',  ( 0.1520645003235147619, 0.2938566582844236441, 0.3972204521082409734 ) ) ;
#17796 = DIRECTION ( 'NONE',  ( -0.000000000000000000, -1.000000000000000000, -0.000000000000000000 ) ) ;
#17797 = ADVANCED_FACE ( 'NONE', ( #7474 ), #15708, .T. ) ;
#17798 = AXIS2_PLACEMENT_3D ( 'NONE', #25248, #11687, #20308 ) ;
#17799 = ORIENTED_EDGE ( 'NONE', *, *, #25329, .T. ) ;
#17800 = LINE ( 'NONE', #15445, #20553 ) ;
#17801 = DIRECTION ( 'NONE',  ( 0.000000000000000000, 0.000000000000000000, 1.000000000000000000 ) ) ;
#17802 = DIRECTION ( 'NONE',  ( -0.4338837391175582314, -0.9009688679024192570, 0.000000000000000000 ) ) ;
#17803 = ORIENTED_EDGE ( 'NONE', *, *, #27799, .T. ) ;
#17804 = CARTESIAN_POINT ( 'NONE',  ( -4.821283464566928349E-18, 0.000000000000000000, -0.2834645669291338543 ) ) ;
#17805 = ORIENTED_EDGE ( 'NONE', *, *, #7949, .F. ) ;
#17807 = EDGE_CURVE ( 'NONE', #6679, #10869, #3093, .T. ) ;
#17806 = AXIS2_PLACEMENT_3D ( 'NONE', #14394, #23005, #24824 ) ;
#17808 = PRESENTATION_STYLE_ASSIGNMENT (( #22755 ) ) ;
#17809 = CIRCLE ( 'NONE', #13310, 0.07677362204724411110 ) ;
#17810 = CARTESIAN_POINT ( 'NONE',  ( 0.8031496062992127261, 0.000000000000000000, 0.02362204724409448786 ) ) ;
#17811 = CARTESIAN_POINT ( 'NONE',  ( 0.7430739993161732393, 0.5308305074509503951, -0.2265429684943779665 ) ) ;
#17812 = EDGE_CURVE ( 'NONE', #21446, #9472, #17066, .T. ) ;
#17813 = CARTESIAN_POINT ( 'NONE',  ( 7.955503286468943460E-18, 0.6102362204724409711, 0.1062972440944881941 ) ) ;
#17814 = FACE_OUTER_BOUND ( 'NONE', #14904, .T. ) ;
#17815 = VERTEX_POINT ( 'NONE', #16509 ) ;
#17816 = CARTESIAN_POINT ( 'NONE',  ( 0.4980314960629921295, 6.099126775281109802E-17, -0.01377952755905511792 ) ) ;
#17817 = CARTESIAN_POINT ( 'NONE',  ( 0.4921259842519685179, -0.03220957031753991784, -1.550196850393700920 ) ) ;
#17818 = EDGE_CURVE ( 'NONE', #18356, #2702, #5797, .T. ) ;
#17819 = CARTESIAN_POINT ( 'NONE',  ( -0.3645739570812778219, -0.2796934465393718927, -1.928289503579152742 ) ) ;
#17820 = CARTESIAN_POINT ( 'NONE',  ( -0.5118110236220472231, 0.000000000000000000, 1.914370078775489148 ) ) ;
#17821 = EDGE_CURVE ( 'NONE', #4552, #25409, #3978, .T. ) ;
#17822 = CARTESIAN_POINT ( 'NONE',  ( 0.6117448998508603353, 0.1083144418130616154, 0.2574819594177531479 ) ) ;
#17823 = DIRECTION ( 'NONE',  ( 0.3174974722037094410, 3.888222630716485107E-17, -0.9482591181445367834 ) ) ;
#17824 = CARTESIAN_POINT ( 'NONE',  ( 0.4921259842519685179, 2.987958743070287587E-17, -1.569881889763779625 ) ) ;
#17825 = CARTESIAN_POINT ( 'NONE',  ( -0.4889536969035324643, 0.06441834428466573781, -1.569881889763779625 ) ) ;
#17826 = ORIENTED_EDGE ( 'NONE', *, *, #19694, .T. ) ;
#17827 = VECTOR ( 'NONE', #22472, 39.37007874015748143 ) ;
#17828 = CARTESIAN_POINT ( 'NONE',  ( -0.6208708315385689236, -0.1269810289789476410, 0.2299899736262448757 ) ) ;
#17829 = CARTESIAN_POINT ( 'NONE',  ( 0.000000000000000000, 0.07874015746264864668, -0.7874015748208159637 ) ) ;
#17830 = DIRECTION ( 'NONE',  ( 0.000000000000000000, -1.000000000000000000, 0.000000000000000000 ) ) ;
#17831 = CARTESIAN_POINT ( 'NONE',  ( 0.4143937130589223639, 0.4928070724598411778, 0.1183902030385255016 ) ) ;
#17832 = CIRCLE ( 'NONE', #2951, 0.01181102362204724393 ) ;
#17833 = CYLINDRICAL_SURFACE ( 'NONE', #21923, 0.4692913385826771866 ) ;
#17834 = CARTESIAN_POINT ( 'NONE',  ( -0.09842519685039370636, 0.07874015748031495954, 0.04546065111729331171 ) ) ;
#17835 = VECTOR ( 'NONE', #27626, 39.37007874015748143 ) ;
#17836 = VERTEX_POINT ( 'NONE', #12129 ) ;
#17837 = CARTESIAN_POINT ( 'NONE',  ( -0.7874015748031496509, 0.4238173070432976197, -0.003642219101859409287 ) ) ;
#17838 = ORIENTED_EDGE ( 'NONE', *, *, #17460, .T. ) ;
#17839 = EDGE_CURVE ( 'NONE', #7282, #11900, #20663, .T. ) ;
#17840 = CARTESIAN_POINT ( 'NONE',  ( 0.4069519308877018182, 0.2006393256663585589, -1.934055118110236338 ) ) ;
#17841 = FACE_OUTER_BOUND ( 'NONE', #14024, .T. ) ;
#17842 = ORIENTED_EDGE ( 'NONE', *, *, #27668, .F. ) ;
#17843 = CARTESIAN_POINT ( 'NONE',  ( -0.002724751885583937862, 0.1704774416898503786, -0.09842519685039353983 ) ) ;
#17844 = EDGE_CURVE ( 'NONE', #24177, #25476, #27395, .T. ) ;
#17845 = CARTESIAN_POINT ( 'NONE',  ( -0.3858850602361762472, -0.2227473777835706492, -1.934055118110236116 ) ) ;
#17846 = CARTESIAN_POINT ( 'NONE',  ( -0.2993674444872340690, 0.2296683860596682170, -3.100567304031764060 ) ) ;
#17847 = DIRECTION ( 'NONE',  ( -0.9749279121818235083, 0.2225209339563148925, 0.000000000000000000 ) ) ;
#17848 = CARTESIAN_POINT ( 'NONE',  ( 0.6117062799105531523, 0.1085321106658064944, 0.2574803149606298969 ) ) ;
#17849 = EDGE_LOOP ( 'NONE', ( #26633, #18764 ) ) ;
#17850 = CARTESIAN_POINT ( 'NONE',  ( 0.4858607088160724063, -0.2805118110236220486, 0.07676968503937006694 ) ) ;
#17851 = AXIS2_PLACEMENT_3D ( 'NONE', #8383, #25472, #6135 ) ;
#17852 = APPLICATION_PROTOCOL_DEFINITION ( 'draft international standard', 'automotive_design', 1998, #17906 ) ;
#17853 = ORIENTED_EDGE ( 'NONE', *, *, #1539, .F. ) ;
#17854 = EDGE_LOOP ( 'NONE', ( #18498, #10342, #1670 ) ) ;
#17855 = CARTESIAN_POINT ( 'NONE',  ( -0.07874015748031495954, 0.04546065111729338803, -0.3779527559055118058 ) ) ;
#17856 = CARTESIAN_POINT ( 'NONE',  ( 0.2952755905264887182, 0.000000000000000000, -4.330708661417323135 ) ) ;
#17857 = CARTESIAN_POINT ( 'NONE',  ( -0.03349795313264251895, -0.5118110236220472231, 1.747047244094488194 ) ) ;
#17858 = ORIENTED_EDGE ( 'NONE', *, *, #9482, .T. ) ;
#17859 = CARTESIAN_POINT ( 'NONE',  ( -0.02438677169350859236, -0.3726024258163779246, -3.115157480314960647 ) ) ;
#17860 = AXIS2_PLACEMENT_3D ( 'NONE', #14938, #19143, #21413 ) ;
#17861 = EDGE_LOOP ( 'NONE', ( #12402, #6756, #17923, #12072 ) ) ;
#17862 = CARTESIAN_POINT ( 'NONE',  ( 0.3334645669291338987, -0.7876517371453680694, -0.8174568431611989316 ) ) ;
#17863 = DIRECTION ( 'NONE',  ( 0.000000000000000000, 0.000000000000000000, -1.000000000000000000 ) ) ;
#17864 = ORIENTED_EDGE ( 'NONE', *, *, #16491, .F. ) ;
#17865 = CARTESIAN_POINT ( 'NONE',  ( 0.04380447413658629385, 0.3324885138898144854, 1.953740157480315043 ) ) ;
#17866 = ORIENTED_EDGE ( 'NONE', *, *, #8957, .F. ) ;
#17867 = ORIENTED_EDGE ( 'NONE', *, *, #20791, .T. ) ;
#17868 = VECTOR ( 'NONE', #15274, 39.37007874015748854 ) ;
#17869 = CARTESIAN_POINT ( 'NONE',  ( 0.0001724821237275781839, 0.3771653543307086909, 0.1992150590373740204 ) ) ;
#17870 = EDGE_LOOP ( 'NONE', ( #13214, #22530 ) ) ;
#17871 = VERTEX_POINT ( 'NONE', #5932 ) ;
#17872 = ORIENTED_EDGE ( 'NONE', *, *, #11071, .F. ) ;
#17873 = CARTESIAN_POINT ( 'NONE',  ( 0.03937007874015747977, 0.000000000000000000, 0.000000000000000000 ) ) ;
#17874 = EDGE_CURVE ( 'NONE', #26931, #26179, #26667, .T. ) ;
#17875 = CARTESIAN_POINT ( 'NONE',  ( -0.3551931031211768008, 0.04679574315772456333, -3.115157480314960647 ) ) ;
#17876 = LINE ( 'NONE', #13944, #404 ) ;
#17877 = DIRECTION ( 'NONE',  ( -1.000000000000000000, 0.000000000000000000, 0.000000000000000000 ) ) ;
#17878 = CARTESIAN_POINT ( 'NONE',  ( 0.01288382813972187464, 0.2165354330708661457, -3.174212598425197207 ) ) ;
#17879 = CARTESIAN_POINT ( 'NONE',  ( 0.04638120790932724613, 0.3520466617656882735, 1.953740157480315043 ) ) ;
#17880 = CARTESIAN_POINT ( 'NONE',  ( -0.1968503937007874127, 0.9448818897637796255, -0.1082677165354330867 ) ) ;
#17881 = AXIS2_PLACEMENT_3D ( 'NONE', #22825, #9955, #5737 ) ;
#17882 = CARTESIAN_POINT ( 'NONE',  ( 0.3223547283257516272, 0.3832433309296771617, 0.09685039370078740717 ) ) ;
#17883 = DIRECTION ( 'NONE',  ( 0.000000000000000000, -1.000000000000000000, 0.000000000000000000 ) ) ;
#17884 = DIRECTION ( 'NONE',  ( 0.000000000000000000, -1.000000000000000000, 0.000000000000000000 ) ) ;
#17885 = FACE_OUTER_BOUND ( 'NONE', #2212, .T. ) ;
#17886 = VERTEX_POINT ( 'NONE', #21177 ) ;
#17887 = EDGE_CURVE ( 'NONE', #3782, #12825, #23165, .T. ) ;
#17888 = FACE_OUTER_BOUND ( 'NONE', #26353, .T. ) ;
#17889 = DIRECTION ( 'NONE',  ( 0.000000000000000000, 0.000000000000000000, 1.000000000000000000 ) ) ;
#17890 = ( NAMED_UNIT ( * ) PLANE_ANGLE_UNIT ( ) SI_UNIT ( $, .RADIAN. ) ) ;
#17891 = VERTEX_POINT ( 'NONE', #25411 ) ;
#17892 = CARTESIAN_POINT ( 'NONE',  ( -0.4716107359529601584, 0.08256389912696107669, 0.1920935997046215038 ) ) ;
#17893 = EDGE_LOOP ( 'NONE', ( #18131, #23583 ) ) ;
#17894 = CARTESIAN_POINT ( 'NONE',  ( 0.3937007874015748254, 0.000000000000000000, -1.934055118110236338 ) ) ;
#17895 = CARTESIAN_POINT ( 'NONE',  ( 0.1522836969735573143, -0.4909267390297480382, -0.05591742528025173131 ) ) ;
#17896 = EDGE_CURVE ( 'NONE', #3406, #12161, #11183, .T. ) ;
#17897 = AXIS2_PLACEMENT_3D ( 'NONE', #20263, #921, #2867 ) ;
#17898 = VERTEX_POINT ( 'NONE', #1267 ) ;
#17899 = CARTESIAN_POINT ( 'NONE',  ( 0.5671862884094760471, 0.07472527936312113594, 0.9399606299212598381 ) ) ;
#17900 = ORIENTED_EDGE ( 'NONE', *, *, #2014, .F. ) ;
#17901 = CARTESIAN_POINT ( 'NONE',  ( 0.3905379133858267737, 0.2805118110236220486, -0.4858607088160732390 ) ) ;
#17902 = CARTESIAN_POINT ( 'NONE',  ( 0.1490609433615242285, 0.4786070381542913421, 0.000000000000000000 ) ) ;
#17903 = CARTESIAN_POINT ( 'NONE',  ( 0.1294857240059045234, -0.3542416573274181357, 0.07637795275590551769 ) ) ;
#17904 = DIRECTION ( 'NONE',  ( -1.000000000000000000, 0.000000000000000000, 0.000000000000000000 ) ) ;
#17905 = CARTESIAN_POINT ( 'NONE',  ( 2.531258147843938596E-16, 0.4724409448818898127, 2.066929133858267598 ) ) ;
#17906 = APPLICATION_CONTEXT ( 'automotive_design' ) ;
#17907 = DIRECTION ( 'NONE',  ( 0.000000000000000000, 0.000000000000000000, -1.000000000000000000 ) ) ;
#17908 = CARTESIAN_POINT ( 'NONE',  ( -0.4068047116067418645, 0.4858504993712711162, 0.2481708550942073044 ) ) ;
#17909 = CARTESIAN_POINT ( 'NONE',  ( -0.07874015748031495954, -0.04546065111729338803, -0.4724409448818898127 ) ) ;
#17910 = CARTESIAN_POINT ( 'NONE',  ( -0.6300376947287432694, -0.09431800512982742302, 0.2327803123842870359 ) ) ;
#17911 = DIRECTION ( 'NONE',  ( -1.000000000000000000, 0.000000000000000000, 0.000000000000000000 ) ) ;
#17912 = AXIS2_PLACEMENT_3D ( 'NONE', #18771, #23031, #23326 ) ;
#17913 = CIRCLE ( 'NONE', #12555, 0.3937007874015748254 ) ;
#17914 = CARTESIAN_POINT ( 'NONE',  ( -0.4055118110236220486, 0.9448818897637796255, -9.561468503937007847E-18 ) ) ;
#17915 = ORIENTED_EDGE ( 'NONE', *, *, #15128, .F. ) ;
#17916 = PRODUCT_DEFINITION_SHAPE ( 'NONE', 'NONE',  #27884 ) ;
#17917 = CARTESIAN_POINT ( 'NONE',  ( 1.197070535079588716, 0.07874015748031495954, -1.197070535079588716 ) ) ;
#17918 = EDGE_CURVE ( 'NONE', #10221, #1935, #20215, .T. ) ;
#17919 = AXIS2_PLACEMENT_3D ( 'NONE', #21792, #13309, #2429 ) ;
#17920 = EDGE_LOOP ( 'NONE', ( #17349, #4935 ) ) ;
#17921 = EDGE_CURVE ( 'NONE', #3819, #3027, #22478, .T. ) ;
#17922 = ADVANCED_FACE ( 'NONE', ( #27257, #7906 ), #1542, .T. ) ;
#17923 = ORIENTED_EDGE ( 'NONE', *, *, #8806, .F. ) ;
#17924 = FACE_OUTER_BOUND ( 'NONE', #24879, .T. ) ;
#17925 = ADVANCED_FACE ( 'NONE', ( #23025 ), #8939, .T. ) ;
#17926 = DIRECTION ( 'NONE',  ( -1.000000000000000000, 0.000000000000000000, 0.000000000000000000 ) ) ;
#17927 = CARTESIAN_POINT ( 'NONE',  ( 0.09586345222253873921, 0.2165354330708661457, -3.573990933995916830 ) ) ;
#17928 = ORIENTED_EDGE ( 'NONE', *, *, #19361, .F. ) ;
#17929 = VERTEX_POINT ( 'NONE', #17485 ) ;
#17930 = DIRECTION ( 'NONE',  ( -1.000000000000000000, 0.000000000000000000, 0.000000000000000000 ) ) ;
#17931 = VECTOR ( 'NONE', #10895, 39.37007874015748854 ) ;
#17932 = CIRCLE ( 'NONE', #18865, 0.6881889763779527325 ) ;
#17933 = CARTESIAN_POINT ( 'NONE',  ( -0.3268939675028499914, -0.1881330340946393564, 0.07637795275590551769 ) ) ;
#17934 = CARTESIAN_POINT ( 'NONE',  ( 0.7872492035923605025, 0.3513616474746652507, 0.02280110086181263637 ) ) ;
#17935 = CARTESIAN_POINT ( 'NONE',  ( 0.3010840436257780639, 0.2313841235333765900, -3.100567304031763616 ) ) ;
#17936 = DIRECTION ( 'NONE',  ( 0.000000000000000000, 0.000000000000000000, -1.000000000000000000 ) ) ;
#17937 = ORIENTED_EDGE ( 'NONE', *, *, #8260, .T. ) ;
#17938 = CARTESIAN_POINT ( 'NONE',  ( 0.09776461103677401565, 0.2994061874507674692, -3.561313241017925790 ) ) ;
#17939 = CARTESIAN_POINT ( 'NONE',  ( -0.2268096725200260955, 0.4600326175569864340, -1.550196850393700920 ) ) ;
#17940 = DIRECTION ( 'NONE',  ( 0.000000000000000000, 1.000000000000000000, 0.000000000000000000 ) ) ;
#17941 = CARTESIAN_POINT ( 'NONE',  ( 0.5230301363771282519, -0.1775991818008710588, 0.9202755905511811330 ) ) ;
#17942 = LINE ( 'NONE', #9479, #13915 ) ;
#17943 = DIRECTION ( 'NONE',  ( -0.000000000000000000, -1.000000000000000000, -0.000000000000000000 ) ) ;
#17944 = CARTESIAN_POINT ( 'NONE',  ( -0.1968503937007874127, -0.07874015748031495954, 0.04546065111729338803 ) ) ;
#17945 = CARTESIAN_POINT ( 'NONE',  ( -0.1477428134820341077, 0.4351030398461640525, -1.928289503579168285 ) ) ;
#17946 = AXIS2_PLACEMENT_3D ( 'NONE', #8051, #17217, #12834 ) ;
#17947 = EDGE_CURVE ( 'NONE', #26700, #11214, #10765, .T. ) ;
#17948 = CARTESIAN_POINT ( 'NONE',  ( 0.3707612262533184766, 0.3252100150720236282, -1.569881889763779625 ) ) ;
#17949 = AXIS2_PLACEMENT_3D ( 'NONE', #9268, #11545, #7447 ) ;
#17950 = CARTESIAN_POINT ( 'NONE',  ( 0.05882388396542066050, 0.8433682279986742802, -0.06931269535625812772 ) ) ;
#17951 = CARTESIAN_POINT ( 'NONE',  ( 0.2181459867426673305, -0.4514914376958676923, 0.1643955689704863221 ) ) ;
#17952 = CYLINDRICAL_SURFACE ( 'NONE', #18111, 0.1771653543307086520 ) ;
#17953 = EDGE_CURVE ( 'NONE', #16188, #724, #35, .T. ) ;
#17954 = CARTESIAN_POINT ( 'NONE',  ( -0.5731455175603529240, -0.3301167833455554423, 0.1616495878887042326 ) ) ;
#17956 = DIRECTION ( 'NONE',  ( -0.000000000000000000, 1.000000000000000000, 0.000000000000000000 ) ) ;
#17955 = CIRCLE ( 'NONE', #1321, 0.6881889763779527325 ) ;
#17957 = CARTESIAN_POINT ( 'NONE',  ( 0.1447526197146039584, -0.3977045540727763839, 0.06102165354330708891 ) ) ;
#17958 = EDGE_LOOP ( 'NONE', ( #252, #24859, #16471, #17463 ) ) ;
#17959 = CARTESIAN_POINT ( 'NONE',  ( 0.5905511811023621549, 4.339299682018180063E-17, 0.3346456692913385988 ) ) ;
#17960 = ORIENTED_EDGE ( 'NONE', *, *, #4364, .T. ) ;
#17961 = CARTESIAN_POINT ( 'NONE',  ( 0.1173917140416251143, -0.4382752542995838052, -1.934055118110236338 ) ) ;
#17962 = CARTESIAN_POINT ( 'NONE',  ( -0.4333114377119193783, -0.2494818589553494115, 0.1496602734600580575 ) ) ;
#17963 = CARTESIAN_POINT ( 'NONE',  ( 0.000000000000000000, 0.000000000000000000, 0.3543307086614173040 ) ) ;
#17964 = CYLINDRICAL_SURFACE ( 'NONE', #12362, 0.09842519685039378963 ) ;
#17965 = CARTESIAN_POINT ( 'NONE',  ( 0.2315507648392299000, -0.4792806379917101678, 0.1322834645669291320 ) ) ;
#17966 = CARTESIAN_POINT ( 'NONE',  ( -0.5182863655200992126, 0.000000000000000000, -0.2204724409448818867 ) ) ;
#17967 = CARTESIAN_POINT ( 'NONE',  ( -0.1141732283464566844, -0.5570866141732283561, 6.822343388950805452E-17 ) ) ;
#17968 = FACE_OUTER_BOUND ( 'NONE', #26843, .T. ) ;
#17969 = VECTOR ( 'NONE', #22205, 39.37007874015748143 ) ;
#17970 = CARTESIAN_POINT ( 'NONE',  ( 0.000000000000000000, 0.9055118110236221041, -0.7874015748031496509 ) ) ;
#17971 = CARTESIAN_POINT ( 'NONE',  ( -0.3535721684717733071, -0.1200583359873110406, -3.115157480314960647 ) ) ;
#17972 = AXIS2_PLACEMENT_3D ( 'NONE', #6379, #10891, #21634 ) ;
#17973 = CARTESIAN_POINT ( 'NONE',  ( -0.06200787401574806013, 7.593774443531818500E-18, 0.7844728274238290666 ) ) ;
#17974 = DIRECTION ( 'NONE',  ( 0.000000000000000000, -1.000000000000000000, 0.000000000000000000 ) ) ;
#17975 = ORIENTED_EDGE ( 'NONE', *, *, #10461, .T. ) ;
#17976 = CARTESIAN_POINT ( 'NONE',  ( -0.3349573549949658169, 0.2938049579018958690, -1.934055118110236338 ) ) ;
#17977 = ADVANCED_FACE ( 'NONE', ( #19621 ), #27004, .F. ) ;
#17978 = EDGE_CURVE ( 'NONE', #21690, #7673, #6480, .T. ) ;
#17979 = EDGE_LOOP ( 'NONE', ( #11527, #4555, #6177, #23122 ) ) ;
#17980 = ADVANCED_FACE ( 'NONE', ( #23988 ), #16638, .T. ) ;
#17981 = ORIENTED_EDGE ( 'NONE', *, *, #14748, .F. ) ;
#17982 = CARTESIAN_POINT ( 'NONE',  ( 0.000000000000000000, 0.000000000000000000, 0.07637795275590551769 ) ) ;
#17983 = CARTESIAN_POINT ( 'NONE',  ( -0.07874015748031489015, 0.000000000000000000, -0.3779527559055118058 ) ) ;
#17984 = CARTESIAN_POINT ( 'NONE',  ( 0.4954415918531143714, 0.1327036767659736105, 1.747047244094488194 ) ) ;
#17985 = EDGE_CURVE ( 'NONE', #7640, #11982, #21135, .T. ) ;
#17986 = FACE_OUTER_BOUND ( 'NONE', #23376, .T. ) ;
#17987 = ORIENTED_EDGE ( 'NONE', *, *, #3120, .T. ) ;
#17988 = CIRCLE ( 'NONE', #15356, 0.1771653543307086798 ) ;
#17989 = CARTESIAN_POINT ( 'NONE',  ( -0.3606853515406215904, -0.09660931395005714628, -3.115157480314960647 ) ) ;
#17990 = CARTESIAN_POINT ( 'NONE',  ( 0.03532354024591842501, -0.6299212598425196763, -0.6299212598425196763 ) ) ;
#17991 = CARTESIAN_POINT ( 'NONE',  ( -2.685748425196850164E-17, 0.000000000000000000, -1.894685039405410665 ) ) ;
#17992 = DIRECTION ( 'NONE',  ( -0.8660254037844382635, 0.5000000000000005551, 0.000000000000000000 ) ) ;
#17993 = ORIENTED_EDGE ( 'NONE', *, *, #26276, .T. ) ;
#17994 = ORIENTED_EDGE ( 'NONE', *, *, #21668, .F. ) ;
#17995 = CARTESIAN_POINT ( 'NONE',  ( -0.3338887748335572225, -0.7960395739734442699, -0.8657810409865404067 ) ) ;
#17996 = CARTESIAN_POINT ( 'NONE',  ( 2.186367668367731174E-17, 0.3771653543307086909, 0.1992150590373740204 ) ) ;
#17997 = VERTEX_POINT ( 'NONE', #25696 ) ;
#17998 = ORIENTED_EDGE ( 'NONE', *, *, #8243, .T. ) ;
#17999 = VERTEX_POINT ( 'NONE', #14979 ) ;
#18000 = CARTESIAN_POINT ( 'NONE',  ( -0.6722178168900768691, 0.05837462721528850068, 0.2350617247236460594 ) ) ;
#18001 = FACE_BOUND ( 'NONE', #24283, .T. ) ;
#18002 = EDGE_CURVE ( 'NONE', #21048, #3293, #22954, .T. ) ;
#18003 = CARTESIAN_POINT ( 'NONE',  ( 0.000000000000000000, 0.000000000000000000, 0.1322834645669291320 ) ) ;
#18004 = CARTESIAN_POINT ( 'NONE',  ( -0.01968503937007873988, 0.000000000000000000, 0.000000000000000000 ) ) ;
#18005 = DIRECTION ( 'NONE',  ( 0.8176200022776350940, 1.001295718708157488E-16, -0.5757582234545329802 ) ) ;
#18006 = VECTOR ( 'NONE', #24282, 39.37007874015748143 ) ;
#18007 = CIRCLE ( 'NONE', #14927, 0.4692913385826771866 ) ;
#18008 = DIRECTION ( 'NONE',  ( 0.000000000000000000, 0.000000000000000000, 1.000000000000000000 ) ) ;
#18009 = CARTESIAN_POINT ( 'NONE',  ( 0.5188885761056504231, -0.1186607836835330693, 0.3401599409343964431 ) ) ;
#18010 = CARTESIAN_POINT ( 'NONE',  ( 0.3074993854542699689, 0.1775730735577541186, 1.953740157480315043 ) ) ;
#18011 = PLANE ( 'NONE',  #8737 ) ;
#18012 = AXIS2_PLACEMENT_3D ( 'NONE', #19676, #8923, #26164 ) ;
#18013 = CARTESIAN_POINT ( 'NONE',  ( 0.000000000000000000, 0.000000000000000000, -0.2755905511811023723 ) ) ;
#18014 = DIRECTION ( 'NONE',  ( -1.000000000000000000, 0.000000000000000000, 0.000000000000000000 ) ) ;
#18015 = FACE_OUTER_BOUND ( 'NONE', #5704, .T. ) ;
#18016 = CARTESIAN_POINT ( 'NONE',  ( -0.2355331214654133032, 0.4777261797697266998, 1.747047244094488194 ) ) ;
#18017 = EDGE_CURVE ( 'NONE', #25955, #1342, #19781, .T. ) ;
#18018 = VERTEX_POINT ( 'NONE', #2507 ) ;
#18019 = EDGE_CURVE ( 'NONE', #9714, #3172, #14397, .T. ) ;
#18020 = CARTESIAN_POINT ( 'NONE',  ( -0.3070866141732283561, 3.760726391082423050E-17, -1.639108858267716421E-17 ) ) ;
#18021 = ORIENTED_EDGE ( 'NONE', *, *, #3062, .T. ) ;
#18022 = CARTESIAN_POINT ( 'NONE',  ( -0.2952755905511810774, 3.688404729715453115E-17, 0.2637795275590551491 ) ) ;
#18023 = ORIENTED_EDGE ( 'NONE', *, *, #15579, .F. ) ;
#18024 = CARTESIAN_POINT ( 'NONE',  ( -0.07217847769028858107, -4.927204724409449161E-18, 0.000000000000000000 ) ) ;
#18025 = VERTEX_POINT ( 'NONE', #21595 ) ;
#18026 = AXIS2_PLACEMENT_3D ( 'NONE', #30, #23981, #4619 ) ;
#18027 = CARTESIAN_POINT ( 'NONE',  ( 0.4270824798167768277, 0.2466292688015001844, -1.569881889763779625 ) ) ;
#18028 = LINE ( 'NONE', #9156, #24180 ) ;
#18029 = ORIENTED_EDGE ( 'NONE', *, *, #1911, .T. ) ;
#18030 = CARTESIAN_POINT ( 'NONE',  ( -0.1839420097223304074, 0.5417097841048854612, 0.9399606299212598381 ) ) ;
#18031 = ORIENTED_EDGE ( 'NONE', *, *, #26551, .T. ) ;
#18032 = CARTESIAN_POINT ( 'NONE',  ( -0.1968503937007874127, 0.1291220684401279684, 0.000000000000000000 ) ) ;
#18033 = DIRECTION ( 'NONE',  ( -1.000000000000000000, 0.000000000000000000, 0.000000000000000000 ) ) ;
#18034 = CONTEXT_DEPENDENT_SHAPE_REPRESENTATION ( #2418, #2808 ) ;
#18035 = LINE ( 'NONE', #24285, #1368 ) ;
#18036 = DIRECTION ( 'NONE',  ( 0.000000000000000000, 0.000000000000000000, 1.000000000000000000 ) ) ;
#18037 = CARTESIAN_POINT ( 'NONE',  ( -0.0007595033562148819414, 0.6881885572739390167, 0.1322834645669291320 ) ) ;
#18038 = CARTESIAN_POINT ( 'NONE',  ( 0.6055690743987126590, -0.2581485381169802973, 0.4471263839182408883 ) ) ;
#18039 = EDGE_CURVE ( 'NONE', #25577, #18698, #23033, .T. ) ;
#18040 = CARTESIAN_POINT ( 'NONE',  ( -0.0004974201395671521515, 0.3464563358313494934, 0.1377952755905512139 ) ) ;
#18041 = DIRECTION ( 'NONE',  ( 1.000000000000000000, 0.000000000000000000, 0.000000000000000000 ) ) ;
#18042 = CARTESIAN_POINT ( 'NONE',  ( -0.2660793235464189999, 0.2041304421298406335, 1.953740157480315043 ) ) ;
#18043 = ORIENTED_EDGE ( 'NONE', *, *, #19368, .F. ) ;
#18044 = CYLINDRICAL_SURFACE ( 'NONE', #19095, 0.1673228346456692994 ) ;
#18045 = LINE ( 'NONE', #14133, #26333 ) ;
#18046 = CIRCLE ( 'NONE', #5924, 0.07677165354330708902 ) ;
#18047 = CARTESIAN_POINT ( 'NONE',  ( 0.000000000000000000, 0.07874015748031508444, -1.377952755905512472 ) ) ;
#18048 = CARTESIAN_POINT ( 'NONE',  ( -0.5118110236220472231, 3.201384367575308305E-17, 1.766732283464566899 ) ) ;
#18049 = B_SPLINE_CURVE_WITH_KNOTS ( 'NONE', 3,
 ( #21538, #12506, #6016, #2185 ),
 .UNSPECIFIED., .F., .F.,
 ( 4, 4 ),
 ( 0.000000000000000000, 1.000000000000000000 ),
 .UNSPECIFIED. ) ;
#18050 = CARTESIAN_POINT ( 'NONE',  ( 0.000000000000000000, 0.000000000000000000, 0.1377952755905511861 ) ) ;
#18051 = CARTESIAN_POINT ( 'NONE',  ( 0.000000000000000000, 0.000000000000000000, -4.370956692913385731E-17 ) ) ;
#18052 = DIRECTION ( 'NONE',  ( -1.000000000000000000, 0.000000000000000000, 0.000000000000000000 ) ) ;
#18053 = ORIENTED_EDGE ( 'NONE', *, *, #6655, .T. ) ;
#18054 = FACE_OUTER_BOUND ( 'NONE', #27815, .T. ) ;
#18055 = CARTESIAN_POINT ( 'NONE',  ( 0.1525037638700916243, -0.2637554987713726651, -0.4194810972668291393 ) ) ;
#18056 = CARTESIAN_POINT ( 'NONE',  ( -0.09842519685039383126, 0.1968503937007873850, -3.548228346456693050 ) ) ;
#18057 = VERTEX_POINT ( 'NONE', #2231 ) ;
#18058 = CARTESIAN_POINT ( 'NONE',  ( 0.000000000000000000, 0.000000000000000000, 0.4488188976377953110 ) ) ;
#18059 = ORIENTED_EDGE ( 'NONE', *, *, #6949, .T. ) ;
#18060 = DIRECTION ( 'NONE',  ( 1.000000000000000000, 0.000000000000000000, 0.000000000000000000 ) ) ;
#18061 = EDGE_CURVE ( 'NONE', #6009, #23041, #18404, .T. ) ;
#18062 = CIRCLE ( 'NONE', #21725, 0.3346456692913385988 ) ;
#18063 = CARTESIAN_POINT ( 'NONE',  ( -0.3002886982018051487, -0.1727973894384557951, 0.1276989850589877462 ) ) ;
#18064 = CARTESIAN_POINT ( 'NONE',  ( 0.5309636003393858328, 0.6336838567619331730, -0.5358812336713733027 ) ) ;
#18065 = EDGE_CURVE ( 'NONE', #21624, #11391, #13863, .T. ) ;
#18066 = VECTOR ( 'NONE', #4878, 39.37007874015748854 ) ;
#18067 = AXIS2_PLACEMENT_3D ( 'NONE', #9237, #11795, #20272 ) ;
#18068 = FACE_OUTER_BOUND ( 'NONE', #16542, .T. ) ;
#18069 = ORIENTED_EDGE ( 'NONE', *, *, #11130, .T. ) ;
#18070 = EDGE_LOOP ( 'NONE', ( #26901, #26566, #24801, #26737, #16755, #17426, #6754, #5166, #1837, #20841, #9524, #16390 ) ) ;
#18071 = CARTESIAN_POINT ( 'NONE',  ( 0.2180862235769456536, -0.4423390553432768879, -1.550196850393700920 ) ) ;
#18072 = ADVANCED_FACE ( 'NONE', ( #7436 ), #23417, .F. ) ;
#18073 = CARTESIAN_POINT ( 'NONE',  ( -0.1286734528930088550, -0.3545375539099149265, 0.1992142436757342316 ) ) ;
#18074 = CARTESIAN_POINT ( 'NONE',  ( 0.5511811023622047445, -0.03607471876262466348, 0.9202755905511811330 ) ) ;
#18075 = FACE_BOUND ( 'NONE', #2662, .T. ) ;
#18076 = EDGE_CURVE ( 'NONE', #9249, #11890, #19339, .T. ) ;
#18077 = CARTESIAN_POINT ( 'NONE',  ( 0.000000000000000000, 0.000000000000000000, 0.1322834645669291320 ) ) ;
#18078 = CARTESIAN_POINT ( 'NONE',  ( 0.5378903297326614874, 0.4292762795476984805, 0.1322810039474933141 ) ) ;
#18079 = CARTESIAN_POINT ( 'NONE',  ( 0.4270824798167768277, 0.2466292688015001844, -1.569881889763779625 ) ) ;
#18080 = DIRECTION ( 'NONE',  ( 0.000000000000000000, 0.000000000000000000, 1.000000000000000000 ) ) ;
#18081 = AXIS2_PLACEMENT_3D ( 'NONE', #3977, #18357, #14449 ) ;
#18082 = DIRECTION ( 'NONE',  ( 0.000000000000000000, 0.000000000000000000, 1.000000000000000000 ) ) ;
#18083 = CARTESIAN_POINT ( 'NONE',  ( 0.2274877609429545866, -0.4708572476026047227, 0.1392975274359326554 ) ) ;
#18084 = CARTESIAN_POINT ( 'NONE',  ( 0.4858607088160724063, -0.2805118110236220486, 0.1771653543307086520 ) ) ;
#18085 = CARTESIAN_POINT ( 'NONE',  ( -0.5383572925355968319, -0.3100567972183898013, 0.09685039370078740717 ) ) ;
#18086 = EDGE_LOOP ( 'NONE', ( #4261, #21512 ) ) ;
#18087 = MECHANICAL_DESIGN_GEOMETRIC_PRESENTATION_REPRESENTATION (  '', ( #27153 ), #18552 ) ;
#18088 = DIRECTION ( 'NONE',  ( 0.000000000000000000, 1.000000000000000000, 0.000000000000000000 ) ) ;
#18089 = FACE_OUTER_BOUND ( 'NONE', #22667, .T. ) ;
#18090 = ORIENTED_EDGE ( 'NONE', *, *, #7701, .F. ) ;
#18091 = CARTESIAN_POINT ( 'NONE',  ( 0.09193127540178998303, 0.3429876364231002062, 1.953740157480315043 ) ) ;
#18092 = ORIENTED_EDGE ( 'NONE', *, *, #1474, .F. ) ;
#18093 = CARTESIAN_POINT ( 'NONE',  ( 0.4382752542996382616, -0.1173917140416361471, -1.934055118110236338 ) ) ;
#18094 = CARTESIAN_POINT ( 'NONE',  ( 0.4333114377119646754, -0.2494818589553824129, 0.1259302777214051094 ) ) ;
#18095 = EDGE_CURVE ( 'NONE', #24094, #27336, #6142, .T. ) ;
#18096 = CARTESIAN_POINT ( 'NONE',  ( -0.4895985792973480133, 0.000000000000000000, -0.09679133858267717494 ) ) ;
#18097 = CARTESIAN_POINT ( 'NONE',  ( 0.3339160553493877859, 9.254566434645669797E-06, -2.341456692880161228 ) ) ;
#18098 = FACE_OUTER_BOUND ( 'NONE', #23263, .T. ) ;
#18099 = B_SPLINE_CURVE_WITH_KNOTS ( 'NONE', 3,
 ( #2680, #3090, #13562, #582, #20066, #15827 ),
 .UNSPECIFIED., .F., .F.,
 ( 4, 2, 4 ),
 ( 0.2291966065698869959, 0.2305109203526899964, 0.2318252341354939960 ),
 .UNSPECIFIED. ) ;
#18100 = DIRECTION ( 'NONE',  ( 0.000000000000000000, 0.000000000000000000, 1.000000000000000000 ) ) ;
#18101 = VERTEX_POINT ( 'NONE', #18295 ) ;
#18102 = VECTOR ( 'NONE', #1489, 39.37007874015748143 ) ;
#18103 = CARTESIAN_POINT ( 'NONE',  ( 0.000000000000000000, 0.8661417322803149910, -0.3937007874015748254 ) ) ;
#18104 = EDGE_CURVE ( 'NONE', #5702, #25047, #21605, .T. ) ;
#18105 = DIRECTION ( 'NONE',  ( 0.000000000000000000, -1.000000000000000000, 0.000000000000000000 ) ) ;
#18106 = CARTESIAN_POINT ( 'NONE',  ( 0.1668516812751446310, 0.3384212623783090512, -3.100567304031764948 ) ) ;
#18107 = PLANE ( 'NONE',  #26477 ) ;
#18108 = EDGE_CURVE ( 'NONE', #14095, #17999, #4379, .T. ) ;
#18109 = ORIENTED_EDGE ( 'NONE', *, *, #3685, .F. ) ;
#18110 = CARTESIAN_POINT ( 'NONE',  ( 0.2938049579018456314, -0.3349573549949907414, -1.934055118110236338 ) ) ;
#18111 = AXIS2_PLACEMENT_3D ( 'NONE', #26587, #13739, #7241 ) ;
#18112 = ( BOUNDED_CURVE ( )  B_SPLINE_CURVE ( 3, ( #2893, #20144, #17347, #8992 ),
 .UNSPECIFIED., .F., .F. ) 
 B_SPLINE_CURVE_WITH_KNOTS ( ( 4, 4 ),
 ( 3.028426401679942259, 3.141592653589793116 ),
 .UNSPECIFIED. ) 
 CURVE ( )  GEOMETRIC_REPRESENTATION_ITEM ( )  RATIONAL_B_SPLINE_CURVE ( ( 1.000000000000000000, 0.9989330679932157953, 0.9989330679932157953, 1.000000000000000000 ) ) 
 REPRESENTATION_ITEM ( '' )  ) ;
#18113 = ADVANCED_FACE ( 'NONE', ( #7031 ), #24727, .T. ) ;
#18114 = CARTESIAN_POINT ( 'NONE',  ( 0.000000000000000000, 0.000000000000000000, 0.6228346456772185791 ) ) ;
#18115 = ORIENTED_EDGE ( 'NONE', *, *, #14908, .F. ) ;
#18116 = CARTESIAN_POINT ( 'NONE',  ( -0.3861436020174326966, -0.7598757196877184983, -0.4401329610783228929 ) ) ;
#18117 = DIRECTION ( 'NONE',  ( 0.000000000000000000, 0.000000000000000000, 1.000000000000000000 ) ) ;
#18118 = CARTESIAN_POINT ( 'NONE',  ( 0.4856708409200641841, -0.1649135259617057481, 1.766732283464566899 ) ) ;
#18119 = CARTESIAN_POINT ( 'NONE',  ( -0.1649135259616916205, -0.4856708409200665155, 1.747047244094488194 ) ) ;
#18120 = CARTESIAN_POINT ( 'NONE',  ( 0.3715251363271980245, 0.06498290224717499786, 0.1992125984251968684 ) ) ;
#18121 = AXIS2_PLACEMENT_3D ( 'NONE', #15349, #24073, #23941 ) ;
#18122 = EDGE_CURVE ( 'NONE', #1802, #11062, #27445, .T. ) ;
#18123 = ORIENTED_EDGE ( 'NONE', *, *, #6805, .F. ) ;
#18124 = AXIS2_PLACEMENT_3D ( 'NONE', #3723, #18977, #1747 ) ;
#18125 = CARTESIAN_POINT ( 'NONE',  ( 0.1668516812751341394, -0.3384212623783144913, -3.100567304031760951 ) ) ;
#18126 = ORIENTED_EDGE ( 'NONE', *, *, #10071, .F. ) ;
#18127 = CARTESIAN_POINT ( 'NONE',  ( -0.6108560151425692641, 1.109681230470063618, -0.06506513713565366397 ) ) ;
#18128 = CARTESIAN_POINT ( 'NONE',  ( -0.2602238532265429005, 0.000000000000000000, 0.07874015748031495954 ) ) ;
#18129 = EDGE_LOOP ( 'NONE', ( #26834, #9618 ) ) ;
#18130 = ORIENTED_EDGE ( 'NONE', *, *, #7947, .T. ) ;
#18131 = ORIENTED_EDGE ( 'NONE', *, *, #14019, .T. ) ;
#18132 = CARTESIAN_POINT ( 'NONE',  ( 0.03359157810797400862, 0.5118096047255845660, -1.550196850393700920 ) ) ;
#18133 = CIRCLE ( 'NONE', #19959, 0.4692913385826771866 ) ;
#18134 = CARTESIAN_POINT ( 'NONE',  ( -0.3338887748335570560, -0.8039705855317598182, -0.9107153245080098491 ) ) ;
#18135 = CARTESIAN_POINT ( 'NONE',  ( -0.4527559055118110520, -0.6889763779527560139, 8.437527159479796553E-17 ) ) ;
#18136 = ORIENTED_EDGE ( 'NONE', *, *, #615, .T. ) ;
#18137 = CARTESIAN_POINT ( 'NONE',  ( 0.4303822302054278182, -0.1152775731717046309, -1.934055118110236338 ) ) ;
#18138 = ORIENTED_EDGE ( 'NONE', *, *, #1415, .T. ) ;
#18139 = CARTESIAN_POINT ( 'NONE',  ( -0.2428345617565149384, 0.2885915454824177218, 0.07637795275590551769 ) ) ;
#18140 = CARTESIAN_POINT ( 'NONE',  ( -0.06881018027188809394, 0.1968503937007874127, -3.587856484193131745 ) ) ;
#18141 = EDGE_CURVE ( 'NONE', #14016, #5387, #17876, .T. ) ;
#18142 = CARTESIAN_POINT ( 'NONE',  ( -0.2490711204941342405, 0.7655264129003995777, -0.7689379837741201484 ) ) ;
#18143 = CARTESIAN_POINT ( 'NONE',  ( 0.03962986251637121149, 0.1968503937007874127, -3.203822249701830494 ) ) ;
#18144 = CARTESIAN_POINT ( 'NONE',  ( 0.07874015748031489015, 0.1968503937007874127, -3.272637795275590733 ) ) ;
#18145 = CARTESIAN_POINT ( 'NONE',  ( 0.2924088307484721261, 0.1685339107540412829, 1.973425196850394192 ) ) ;
#18146 = CARTESIAN_POINT ( 'NONE',  ( -0.8267716535433071723, 1.012503259137575512E-16, 0.4488188976377953110 ) ) ;
#18147 = PRODUCT_DEFINITION_SHAPE ( 'NONE', 'NONE',  #27898 ) ;
#18148 = ADVANCED_FACE ( 'NONE', ( #3038 ), #3054, .F. ) ;
#18149 = AXIS2_PLACEMENT_3D ( 'NONE', #25158, #3979, #12031 ) ;
#18150 = DIRECTION ( 'NONE',  ( 0.000000000000000000, 0.000000000000000000, 1.000000000000000000 ) ) ;
#18151 = DIRECTION ( 'NONE',  ( -1.000000000000000000, 0.000000000000000000, 0.000000000000000000 ) ) ;
#18152 = DIRECTION ( 'NONE',  ( 0.000000000000000000, 0.000000000000000000, 1.000000000000000000 ) ) ;
#18153 = CARTESIAN_POINT ( 'NONE',  ( -0.2341512108694372152, -0.2669480828848191933, 1.953740157480315043 ) ) ;
#18154 = ADVANCED_FACE ( 'NONE', ( #19886 ), #16177, .T. ) ;
#18155 = ORIENTED_EDGE ( 'NONE', *, *, #24024, .T. ) ;
#18156 = CARTESIAN_POINT ( 'NONE',  ( -0.5381367953593149123, -0.3104394140547397374, 0.2574827755769819038 ) ) ;
#18157 = CIRCLE ( 'NONE', #6024, 0.06889763779527552368 ) ;
#18158 = DIRECTION ( 'NONE',  ( 1.000000000000000000, 0.000000000000000000, 0.000000000000000000 ) ) ;
#18159 = CARTESIAN_POINT ( 'NONE',  ( -0.05118110236220472370, -0.5570866141732283561, 6.822343388950805452E-17 ) ) ;
#18160 = CIRCLE ( 'NONE', #6489, 0.3937007874015748254 ) ;
#18161 = CYLINDRICAL_SURFACE ( 'NONE', #12855, 0.6881889763779527325 ) ;
#18162 = CARTESIAN_POINT ( 'NONE',  ( -0.3512268162760389667, -0.4004221243553605092, 1.747047244094488194 ) ) ;
#18163 = AXIS2_PLACEMENT_3D ( 'NONE', #18570, #9537, #11812 ) ;
#18164 = ORIENTED_EDGE ( 'NONE', *, *, #16318, .F. ) ;
#18165 = PLANE ( 'NONE',  #22801 ) ;
#18166 = ORIENTED_EDGE ( 'NONE', *, *, #7420, .F. ) ;
#18167 = CARTESIAN_POINT ( 'NONE',  ( 0.4165721057576322606, 0.3313508221749649763, 0.1322834645669291320 ) ) ;
#18168 = CARTESIAN_POINT ( 'NONE',  ( 0.000000000000000000, 0.000000000000000000, -0.1111195235210984261 ) ) ;
#18169 = ( NAMED_UNIT ( * ) PLANE_ANGLE_UNIT ( ) SI_UNIT ( $, .RADIAN. ) ) ;
#18170 = CLOSED_SHELL ( 'NONE', ( #3969, #15255, #3574, #19135, #14106, #6549, #6081, #20940, #26660, #18154, #27265, #22637, #16787, #10845, #13526, #26597, #12854, #27332, #20536, #26158, #23647, #9017, #6298, #9983, #21250, #24871, #6838, #21094, #22058, #15572, #13551, #23779, #16396, #20024, #13703, #13552, #24739, #2415 ) ) ;
#18171 = CARTESIAN_POINT ( 'NONE',  ( 0.03532354024591720376, -0.8267716535433071723, 0.000000000000000000 ) ) ;
#18172 = ORIENTED_EDGE ( 'NONE', *, *, #1366, .T. ) ;
#18173 = AXIS2_PLACEMENT_3D ( 'NONE', #13497, #2625, #11250 ) ;
#18174 = CARTESIAN_POINT ( 'NONE',  ( 0.4423390553432409722, -0.2180862235769587265, -1.569881889763779625 ) ) ;
#18175 = ORIENTED_EDGE ( 'NONE', *, *, #7763, .T. ) ;
#18176 = CARTESIAN_POINT ( 'NONE',  ( -0.3772436174784328244, 0.4300830224589641260, 0.9399606299212598381 ) ) ;
#18177 = VERTEX_POINT ( 'NONE', #22556 ) ;
#18178 = DIRECTION ( 'NONE',  ( 0.000000000000000000, 0.000000000000000000, -1.000000000000000000 ) ) ;
#18180 = EDGE_CURVE ( 'NONE', #22130, #4351, #11463, .T. ) ;
#18179 = AXIS2_PLACEMENT_3D ( 'NONE', #16213, #24816, #20588 ) ;
#18181 = DIRECTION ( 'NONE',  ( 0.000000000000000000, 1.000000000000000000, 0.000000000000000000 ) ) ;
#18182 = CONTEXT_DEPENDENT_SHAPE_REPRESENTATION ( #26752, #20436 ) ;
#18183 = CARTESIAN_POINT ( 'NONE',  ( 0.1501355178992943018, 0.4826710871606305076, -0.03296692058268119868 ) ) ;
#18184 = CARTESIAN_POINT ( 'NONE',  ( -0.1580799066051628565, -0.4326553680327470675, 0.1903859678385282639 ) ) ;
#18185 = CYLINDRICAL_SURFACE ( 'NONE', #7307, 0.5531496062992126150 ) ;
#18186 = CARTESIAN_POINT ( 'NONE',  ( -0.2602238532265429005, 0.000000000000000000, 0.2362204724409449064 ) ) ;
#18187 = ORIENTED_EDGE ( 'NONE', *, *, #6583, .F. ) ;
#18188 = DIRECTION ( 'NONE',  ( 1.000000000000000000, 0.000000000000000000, 0.000000000000000000 ) ) ;
#18189 = EDGE_CURVE ( 'NONE', #4754, #27858, #17522, .T. ) ;
#18190 = ADVANCED_FACE ( 'NONE', ( #7730 ), #27083, .T. ) ;
#18191 = DIRECTION ( 'NONE',  ( 0.000000000000000000, 0.000000000000000000, 1.000000000000000000 ) ) ;
#18192 = AXIS2_PLACEMENT_3D ( 'NONE', #17536, #13150, #21777 ) ;
#18193 = CARTESIAN_POINT ( 'NONE',  ( -0.1968503937007874127, -0.4724409448818898127, -0.8182917201112815953 ) ) ;
#18194 = VERTEX_POINT ( 'NONE', #1504 ) ;
#18195 = FACE_OUTER_BOUND ( 'NONE', #5165, .T. ) ;
#18196 = CARTESIAN_POINT ( 'NONE',  ( 0.1516263115863346334, 0.4909405214979283838, -0.05579628926458630317 ) ) ;
#18197 = CARTESIAN_POINT ( 'NONE',  ( -0.6108456259501230390, -0.1623518946918469374, 0.2259549200537961378 ) ) ;
#18198 = CARTESIAN_POINT ( 'NONE',  ( 0.000000000000000000, 0.000000000000000000, 0.3401574803149606252 ) ) ;
#18199 = CARTESIAN_POINT ( 'NONE',  ( 0.000000000000000000, 0.000000000000000000, -0.4724409448818898127 ) ) ;
#18200 = DIRECTION ( 'NONE',  ( 0.1736481776669299426, -0.9848077530122081313, 0.000000000000000000 ) ) ;
#18201 = DIRECTION ( 'NONE',  ( 0.000000000000000000, 0.000000000000000000, 1.000000000000000000 ) ) ;
#18202 = CIRCLE ( 'NONE', #11917, 0.3771653543307086909 ) ;
#18203 = ORIENTED_EDGE ( 'NONE', *, *, #4865, .F. ) ;
#18204 = CIRCLE ( 'NONE', #2878, 0.7874015748208159637 ) ;
#18205 = ( NAMED_UNIT ( * ) PLANE_ANGLE_UNIT ( ) SI_UNIT ( $, .RADIAN. ) ) ;
#18206 = ORIENTED_EDGE ( 'NONE', *, *, #12492, .F. ) ;
#18207 = DIRECTION ( 'NONE',  ( 0.000000000000000000, 1.000000000000000000, 0.000000000000000000 ) ) ;
#18208 = DIRECTION ( 'NONE',  ( 0.000000000000000000, 0.000000000000000000, 1.000000000000000000 ) ) ;
#18209 = CARTESIAN_POINT ( 'NONE',  ( 0.04956879678466356159, 0.1968503937007203553, -3.634230943941128888 ) ) ;
#18210 = VERTEX_POINT ( 'NONE', #27362 ) ;
#18211 = CARTESIAN_POINT ( 'NONE',  ( -0.5118110236220473341, 0.000000000000000000, -1.550196850393700920 ) ) ;
#18212 = CIRCLE ( 'NONE', #1114, 0.4267795243146149664 ) ;
#18213 = CARTESIAN_POINT ( 'NONE',  ( -0.07874015748031495954, 0.1968503937007874127, -3.456364829396325611 ) ) ;
#18214 = ORIENTED_EDGE ( 'NONE', *, *, #9320, .F. ) ;
#18215 = EDGE_CURVE ( 'NONE', #16146, #12126, #25373, .T. ) ;
#18216 = CARTESIAN_POINT ( 'NONE',  ( -0.3020416211876971735, -0.1738080303460615705, 0.1166443193931544220 ) ) ;
#18217 = CARTESIAN_POINT ( 'NONE',  ( 0.6175000359513720394, 0.9054199137833151001, -0.1265032560721565114 ) ) ;
#18218 = EDGE_CURVE ( 'NONE', #17310, #19062, #1292, .T. ) ;
#18219 = AXIS2_PLACEMENT_3D ( 'NONE', #17091, #23332, #3956 ) ;
#18220 = DIRECTION ( 'NONE',  ( -1.000000000000000000, 0.000000000000000000, 0.000000000000000000 ) ) ;
#18221 = CARTESIAN_POINT ( 'NONE',  ( -0.2303471512294322787, -0.4798602677570401598, 0.3401574803149606252 ) ) ;
#18222 = CIRCLE ( 'NONE', #8774, 0.4692913385826771866 ) ;
#18223 = VERTEX_POINT ( 'NONE', #8012 ) ;
#18224 = ORIENTED_EDGE ( 'NONE', *, *, #25231, .T. ) ;
#18225 = CARTESIAN_POINT ( 'NONE',  ( 0.3346456692913385988, 0.02190250779246873461, 1.973425196850393970 ) ) ;
#18226 = CARTESIAN_POINT ( 'NONE',  ( -0.2775852647713619725, 0.4816145447621894005, 0.9202755905511812440 ) ) ;
#18227 = CARTESIAN_POINT ( 'NONE',  ( -0.3362148458988027944, 0.4382482975805537806, 0.9399606299212598381 ) ) ;
#18228 = CARTESIAN_POINT ( 'NONE',  ( -0.1141732283464566844, -0.7539370078740157410, 9.233065434516462138E-17 ) ) ;
#18229 = FACE_OUTER_BOUND ( 'NONE', #17097, .T. ) ;
#18230 = ORIENTED_EDGE ( 'NONE', *, *, #10686, .T. ) ;
#18231 = CARTESIAN_POINT ( 'NONE',  ( -0.4164331889188472857, 0.3315254675241992577, 0.3401591244667909186 ) ) ;
#18232 = CIRCLE ( 'NONE', #677, 0.1298643763538141760 ) ;
#18233 = CARTESIAN_POINT ( 'NONE',  ( -0.4669911931914806358, 0.1585706980422473544, -1.569881889763779625 ) ) ;
#18234 = DIRECTION ( 'NONE',  ( 0.000000000000000000, -1.000000000000000000, 0.000000000000000000 ) ) ;
#18235 = DIRECTION ( 'NONE',  ( 1.000000000000000000, 0.000000000000000000, 0.000000000000000000 ) ) ;
#18236 = CARTESIAN_POINT ( 'NONE',  ( 0.1714649452450068834, -0.4705186852026070898, 0.2574827755769819038 ) ) ;
#18237 = EDGE_CURVE ( 'NONE', #7963, #280, #10394, .T. ) ;
#18238 = CARTESIAN_POINT ( 'NONE',  ( 0.2315507648392299000, -0.4792806379917101678, 0.1322834645669291320 ) ) ;
#18239 = ORIENTED_EDGE ( 'NONE', *, *, #21609, .F. ) ;
#18240 = EDGE_CURVE ( 'NONE', #9314, #10270, #12113, .T. ) ;
#18241 = CIRCLE ( 'NONE', #2901, 0.2952755905511810774 ) ;
#18242 = LENGTH_MEASURE_WITH_UNIT ( LENGTH_MEASURE( 0.02539999999999999897 ), #11764 ) ;
#18243 = PRODUCT_DEFINITION ( 'UNKNOWN', '', #9291, #23524 ) ;
#18244 = CIRCLE ( 'NONE', #5171, 1.377952755905512472 ) ;
#18245 = FACE_BOUND ( 'NONE', #5666, .T. ) ;
#18246 = DIRECTION ( 'NONE',  ( 1.000000000000000000, 0.000000000000000000, 0.000000000000000000 ) ) ;
#18247 = ORIENTED_EDGE ( 'NONE', *, *, #17807, .T. ) ;
#18248 = DIRECTION ( 'NONE',  ( 0.000000000000000000, 0.000000000000000000, -1.000000000000000000 ) ) ;
#18249 = ORIENTED_EDGE ( 'NONE', *, *, #5314, .F. ) ;
#18250 = CARTESIAN_POINT ( 'NONE',  ( 0.0006620872580293073444, 0.5229309616560341434, 0.3331434174597993625 ) ) ;
#18251 = DIRECTION ( 'NONE',  ( 0.000000000000000000, 0.000000000000000000, -1.000000000000000000 ) ) ;
#18252 = EDGE_CURVE ( 'NONE', #20698, #24921, #3527, .T. ) ;
#18253 = DIRECTION ( 'NONE',  ( 0.000000000000000000, 0.000000000000000000, 1.000000000000000000 ) ) ;
#18254 = DIRECTION ( 'NONE',  ( 1.000000000000000000, 0.000000000000000000, 0.000000000000000000 ) ) ;
#18255 = ORIENTED_EDGE ( 'NONE', *, *, #3464, .T. ) ;
#18256 = CIRCLE ( 'NONE', #17400, 0.1003956692913385712 ) ;
#18257 = FACE_OUTER_BOUND ( 'NONE', #493, .T. ) ;
#18258 = CARTESIAN_POINT ( 'NONE',  ( -0.2089723435111590921, -0.4324731448915377641, 0.2362204724409450174 ) ) ;
#18259 = ORIENTED_EDGE ( 'NONE', *, *, #15606, .F. ) ;
#18260 = CARTESIAN_POINT ( 'NONE',  ( -0.02464264302293797324, 0.3765118517642104257, -3.100567304031763172 ) ) ;
#18261 = FACE_OUTER_BOUND ( 'NONE', #27492, .T. ) ;
#18262 = EDGE_LOOP ( 'NONE', ( #21858, #25085, #26918, #10708, #25496, #13851 ) ) ;
#18263 = CARTESIAN_POINT ( 'NONE',  ( 0.4218945342797220666, 0.1432577568504696530, -1.934055118110236338 ) ) ;
#18264 = AXIS2_PLACEMENT_3D ( 'NONE', #23785, #12889, #17136 ) ;
#18265 = AXIS2_PLACEMENT_3D ( 'NONE', #9168, #707, #26143 ) ;
#18266 = SHAPE_DEFINITION_REPRESENTATION ( #12273, #9188 ) ;
#18267 = ADVANCED_FACE ( 'NONE', ( #25232 ), #421, .F. ) ;
#18268 = B_SPLINE_CURVE_WITH_KNOTS ( 'NONE', 3,
 ( #4959, #18213, #24725, #1156 ),
 .UNSPECIFIED., .F., .F.,
 ( 4, 4 ),
 ( 0.000000000000000000, 1.000000000000000000 ),
 .UNSPECIFIED. ) ;
#18269 = FACE_OUTER_BOUND ( 'NONE', #11592, .T. ) ;
#18270 = DIRECTION ( 'NONE',  ( -0.000000000000000000, 1.000000000000000000, -0.000000000000000000 ) ) ;
#18271 = CARTESIAN_POINT ( 'NONE',  ( 0.5085118447801136865, 0.06699507805368522251, 1.747047244094488194 ) ) ;
#18272 = EDGE_CURVE ( 'NONE', #17082, #4219, #19013, .T. ) ;
#18273 = AXIS2_PLACEMENT_3D ( 'NONE', #10375, #23674, #3887 ) ;
#18274 = ORIENTED_EDGE ( 'NONE', *, *, #3993, .F. ) ;
#18275 = SURFACE_STYLE_FILL_AREA ( #20133 ) ;
#18276 = ORIENTED_EDGE ( 'NONE', *, *, #27662, .T. ) ;
#18277 = EDGE_CURVE ( 'NONE', #25, #10350, #5049, .T. ) ;
#18278 = CARTESIAN_POINT ( 'NONE',  ( 0.3740848232703729015, -0.04928467685644277729, -3.100567304031765392 ) ) ;
#18279 = VERTEX_POINT ( 'NONE', #27508 ) ;
#18280 = CARTESIAN_POINT ( 'NONE',  ( 0.7874015748031497619, 0.3447235678987860541, 0.02357451147970114971 ) ) ;
#18281 = CARTESIAN_POINT ( 'NONE',  ( -0.08294224740493445769, -0.3759928968107512648, 0.2015410452432984389 ) ) ;
#18282 = EDGE_CURVE ( 'NONE', #21391, #23447, #6722, .T. ) ;
#18283 = CARTESIAN_POINT ( 'NONE',  ( -0.3361686847406328282, -0.7841026825723664828, -0.8202046661941250205 ) ) ;
#18284 = DIRECTION ( 'NONE',  ( -1.000000000000000000, 0.000000000000000000, 0.000000000000000000 ) ) ;
#18285 = EDGE_CURVE ( 'NONE', #18599, #2223, #4480, .T. ) ;
#18286 = AXIS2_PLACEMENT_3D ( 'NONE', #9734, #5509, #15959 ) ;
#18287 = ORIENTED_EDGE ( 'NONE', *, *, #1786, .F. ) ;
#18288 = VERTEX_POINT ( 'NONE', #1780 ) ;
#18289 = CARTESIAN_POINT ( 'NONE',  ( 0.0002221395201540944610, 0.5322834645669292097, 0.3401599409343964431 ) ) ;
#18290 = CARTESIAN_POINT ( 'NONE',  ( -1.928513779527558736E-17, 0.000000000000000000, -0.4448818897637791814 ) ) ;
#18291 = AXIS2_PLACEMENT_3D ( 'NONE', #18193, #15565, #24227 ) ;
#18292 = B_SPLINE_CURVE_WITH_KNOTS ( 'NONE', 3,
 ( #16485, #8301, #16770, #17053, #14387, #18873 ),
 .UNSPECIFIED., .F., .F.,
 ( 4, 2, 4 ),
 ( 0.5000000000000000000, 0.7500000000000000000, 1.000000000000000000 ),
 .UNSPECIFIED. ) ;
#18293 = EDGE_CURVE ( 'NONE', #25047, #11425, #23433, .T. ) ;
#18294 = FACE_OUTER_BOUND ( 'NONE', #12686, .T. ) ;
#18295 = CARTESIAN_POINT ( 'NONE',  ( 0.5905511811023621549, 0.000000000000000000, 1.707677165389662743 ) ) ;
#18296 = CARTESIAN_POINT ( 'NONE',  ( -9.506830708661417994E-16, -1.653543307086614345, 1.012503259137575512E-16 ) ) ;
#18297 = CARTESIAN_POINT ( 'NONE',  ( -0.2131049448084480213, -0.5835666837866708700, 0.2574803149606298969 ) ) ;
#18298 = CARTESIAN_POINT ( 'NONE',  ( 0.000000000000000000, 0.000000000000000000, -0.1111195235210984261 ) ) ;
#18299 = CARTESIAN_POINT ( 'NONE',  ( -0.2056553984168023042, -0.2676050456844303871, 1.973425196850394636 ) ) ;
#18300 = CARTESIAN_POINT ( 'NONE',  ( 0.3074993854542625304, -0.1775730735577552566, 1.953740157480315043 ) ) ;
#18301 = VERTEX_POINT ( 'NONE', #5756 ) ;
#18302 = FACE_OUTER_BOUND ( 'NONE', #7008, .T. ) ;
#18303 = CARTESIAN_POINT ( 'NONE',  ( -0.5381367953593070297, -0.3104394140547547809, 0.09684793308443542803 ) ) ;
#18304 = DIRECTION ( 'NONE',  ( -1.000000000000000000, 0.000000000000000000, 0.000000000000000000 ) ) ;
#18305 = CARTESIAN_POINT ( 'NONE',  ( -0.5811915241081616612, -0.4724399524670138684, 0.9954595399565421276 ) ) ;
#18306 = CARTESIAN_POINT ( 'NONE',  ( 0.2982299571078434464, 0.3545282230955180136, 0.2048502514855274625 ) ) ;
#18307 = AXIS2_PLACEMENT_3D ( 'NONE', #17376, #1843, #27704 ) ;
#18308 = DIRECTION ( 'NONE',  ( 0.9396926207859082059, -0.3420201433256690460, 0.000000000000000000 ) ) ;
#18309 = CARTESIAN_POINT ( 'NONE',  ( 0.1378076643338917162, 0.5144970376936037759, 1.747047244094488194 ) ) ;
#18310 = CARTESIAN_POINT ( 'NONE',  ( -0.4856708409200606313, -0.1649135259617140470, 1.766732283464566899 ) ) ;
#18311 = ORIENTED_EDGE ( 'NONE', *, *, #7754, .T. ) ;
#18312 = AXIS2_PLACEMENT_3D ( 'NONE', #12615, #25177, #12325 ) ;
#18313 = ORIENTED_EDGE ( 'NONE', *, *, #27270, .T. ) ;
#18314 = CARTESIAN_POINT ( 'NONE',  ( -0.2842490391651705806, 0.2180698645301660521, -3.115157480314960647 ) ) ;
#18315 = ORIENTED_EDGE ( 'NONE', *, *, #27546, .T. ) ;
#18316 = CARTESIAN_POINT ( 'NONE',  ( 0.5981657849660177995, 0.2403521948818893861, -0.4163022132461299263 ) ) ;
#18317 = CARTESIAN_POINT ( 'NONE',  ( -0.4218945342797432163, 0.1432577568504689591, -1.934055118110236338 ) ) ;
#18318 = FACE_OUTER_BOUND ( 'NONE', #8997, .T. ) ;
#18319 = EDGE_CURVE ( 'NONE', #6332, #19539, #8094, .T. ) ;
#18320 = CARTESIAN_POINT ( 'NONE',  ( 0.2997912780622382090, -0.1736589463928937538, 0.1377952755905513249 ) ) ;
#18321 = VERTEX_POINT ( 'NONE', #11466 ) ;
#18322 = ORIENTED_EDGE ( 'NONE', *, *, #6699, .F. ) ;
#18323 = CARTESIAN_POINT ( 'NONE',  ( 0.3252100150720381722, -0.3707612262533039327, -1.569881889763779625 ) ) ;
#18324 = VERTEX_POINT ( 'NONE', #17813 ) ;
#18325 = ORIENTED_EDGE ( 'NONE', *, *, #6361, .F. ) ;
#18326 = CARTESIAN_POINT ( 'NONE',  ( -0.5072939182192724994, -0.3381818976696540080, -0.3094365891633428789 ) ) ;
#18327 = VECTOR ( 'NONE', #15357, 39.37007874015748143 ) ;
#18328 = B_SPLINE_CURVE_WITH_KNOTS ( 'NONE', 3,
 ( #15669, #2657, #22152, #24001, #4637, #2245, #19900, #25988 ),
 .UNSPECIFIED., .F., .F.,
 ( 4, 2, 2, 4 ),
 ( 0.5000000000000000000, 0.7499999999999998890, 0.8750000000000000000, 1.000000000000000000 ),
 .UNSPECIFIED. ) ;
#18329 = CARTESIAN_POINT ( 'NONE',  ( 0.5981657849660177995, 0.000000000000000000, 0.000000000000000000 ) ) ;
#18330 = DIRECTION ( 'NONE',  ( 0.000000000000000000, 0.000000000000000000, 1.000000000000000000 ) ) ;
#18331 = CARTESIAN_POINT ( 'NONE',  ( 0.4167985568850881561, 0.07349283109919289847, 0.2145688976377952695 ) ) ;
#18332 = EDGE_CURVE ( 'NONE', #14583, #20609, #2211, .T. ) ;
#18333 = AXIS2_PLACEMENT_3D ( 'NONE', #22701, #2031, #10643 ) ;
#18334 = CARTESIAN_POINT ( 'NONE',  ( -0.1180276236025431524, -0.3257325899126714552, 0.1377952755905512139 ) ) ;
#18335 = UNCERTAINTY_MEASURE_WITH_UNIT (LENGTH_MEASURE( 1.000000000000000082E-05 ), #27464, 'distance_accuracy_value', 'NONE') ;
#18336 = EDGE_LOOP ( 'NONE', ( #59, #21864, #8408, #23427 ) ) ;
#18337 = CARTESIAN_POINT ( 'NONE',  ( 0.000000000000000000, 0.000000000000000000, 0.1377952755905511861 ) ) ;
#18338 = CARTESIAN_POINT ( 'NONE',  ( -0.3073078020560655044, 0.3671449284694313087, 0.08349695147664858152 ) ) ;
#18339 = CARTESIAN_POINT ( 'NONE',  ( -0.6098875082770396361, -0.1657139659499494710, 0.2255226463234533685 ) ) ;
#18340 = CARTESIAN_POINT ( 'NONE',  ( 0.000000000000000000, -0.1136516277932328595, -0.1968503937007874127 ) ) ;
#18341 = CARTESIAN_POINT ( 'NONE',  ( -0.2350342994816159436, 0.2808987121518214392, 0.08455817588142111596 ) ) ;
#18342 = PLANE ( 'NONE',  #25014 ) ;
#18343 = ( BOUNDED_CURVE ( )  B_SPLINE_CURVE ( 2, ( #22151, #11413, #24539 ),
 .UNSPECIFIED., .F., .F. ) 
 B_SPLINE_CURVE_WITH_KNOTS ( ( 3, 3 ),
 ( 0.000000000000000000, 0.5842180690389598974 ),
 .UNSPECIFIED. ) 
 CURVE ( )  GEOMETRIC_REPRESENTATION_ITEM ( )  RATIONAL_B_SPLINE_CURVE ( ( 1.000000000000000000, 1.154700538379249908, 1.000000000000000000 ) ) 
 REPRESENTATION_ITEM ( '' )  ) ;
#18344 = DIRECTION ( 'NONE',  ( 0.000000000000000000, 1.000000000000000000, 0.000000000000000000 ) ) ;
#18345 = ADVANCED_FACE ( 'NONE', ( #13579, #6312 ), #22201, .T. ) ;
#18346 = DIRECTION ( 'NONE',  ( 0.000000000000000000, 1.000000000000000000, 0.000000000000000000 ) ) ;
#18347 = VERTEX_POINT ( 'NONE', #7097 ) ;
#18348 = EDGE_CURVE ( 'NONE', #5829, #5072, #8471, .T. ) ;
#18349 = ORIENTED_EDGE ( 'NONE', *, *, #21190, .T. ) ;
#18350 = CIRCLE ( 'NONE', #20620, 0.6212598425196850238 ) ;
#18351 = DIRECTION ( 'NONE',  ( 1.000000000000000000, -1.147443000000000016E-15, 0.000000000000000000 ) ) ;
#18352 = LINE ( 'NONE', #9462, #26106 ) ;
#18353 = B_SPLINE_CURVE_WITH_KNOTS ( 'NONE', 3,
 ( #7310, #13521, #424, #26800, #13811, #22016 ),
 .UNSPECIFIED., .F., .F.,
 ( 4, 2, 4 ),
 ( 0.3108507187342950395, 0.3125269569790670166, 0.3142031952238389936 ),
 .UNSPECIFIED. ) ;
#18354 = CARTESIAN_POINT ( 'NONE',  ( 0.06880207798751825088, 0.1968503937007873850, -3.587883383884366229 ) ) ;
#18355 = FACE_OUTER_BOUND ( 'NONE', #14065, .T. ) ;
#18356 = VERTEX_POINT ( 'NONE', #14943 ) ;
#18357 = DIRECTION ( 'NONE',  ( -1.000000000000000000, 0.000000000000000000, 0.000000000000000000 ) ) ;
#18358 = DIRECTION ( 'NONE',  ( 0.000000000000000000, 0.000000000000000000, 1.000000000000000000 ) ) ;
#18359 = EDGE_LOOP ( 'NONE', ( #15348, #22961 ) ) ;
#18360 = CARTESIAN_POINT ( 'NONE',  ( -0.6241612306976536129, 0.1093779649445508623, 0.1061598535652353986 ) ) ;
#18361 = ORIENTED_EDGE ( 'NONE', *, *, #24424, .T. ) ;
#18362 = CIRCLE ( 'NONE', #20177, 0.1299232283464566984 ) ;
#18363 = CARTESIAN_POINT ( 'NONE',  ( -0.2660793235464223860, 0.2041304421298429095, 1.973425196850393970 ) ) ;
#18364 = DIRECTION ( 'NONE',  ( 0.000000000000000000, 0.000000000000000000, 1.000000000000000000 ) ) ;
#18365 = AXIS2_PLACEMENT_3D ( 'NONE', #19416, #25778, #15469 ) ;
#18366 = CARTESIAN_POINT ( 'NONE',  ( 0.5335524835332358107, -0.1429116519061119361, 0.9202755905511811330 ) ) ;
#18367 = LINE ( 'NONE', #18228, #18862 ) ;
#18368 = DIRECTION ( 'NONE',  ( 0.000000000000000000, 0.000000000000000000, 1.000000000000000000 ) ) ;
#18369 = ORIENTED_EDGE ( 'NONE', *, *, #26988, .F. ) ;
#18370 = DIRECTION ( 'NONE',  ( 1.224646799147353207E-16, 1.000000000000000000, -0.000000000000000000 ) ) ;
#18371 = CARTESIAN_POINT ( 'NONE',  ( 0.2180862235769582824, 0.4423390553432410832, -1.569881889763779625 ) ) ;
#18372 = ( LENGTH_UNIT ( ) NAMED_UNIT ( * ) SI_UNIT ( $, .METRE. ) ) ;
#18373 = ORIENTED_EDGE ( 'NONE', *, *, #7491, .T. ) ;
#18374 = B_SPLINE_CURVE_WITH_KNOTS ( 'NONE', 3,
 ( #24691, #15680, #15813, #15951, #9161, #20183 ),
 .UNSPECIFIED., .F., .F.,
 ( 4, 2, 4 ),
 ( 0.5000000000000000000, 0.7500000000000000000, 1.000000000000000000 ),
 .UNSPECIFIED. ) ;
#18375 = CARTESIAN_POINT ( 'NONE',  ( 0.4895462770359960136, 1.042587244177305195, -0.2949132003431571003 ) ) ;
#18376 = CARTESIAN_POINT ( 'NONE',  ( -0.03488411621188159534, 0.5314946440730492494, 1.747047244094488638 ) ) ;
#18377 = CARTESIAN_POINT ( 'NONE',  ( 0.6202606299212598540, -0.08876456692913387014, 0.000000000000000000 ) ) ;
#18378 = DIRECTION ( 'NONE',  ( 0.000000000000000000, 0.000000000000000000, -1.000000000000000000 ) ) ;
#18379 = EDGE_CURVE ( 'NONE', #12220, #9015, #17541, .T. ) ;
#18380 = AXIS2_PLACEMENT_3D ( 'NONE', #17247, #15144, #12999 ) ;
#18381 = ORIENTED_EDGE ( 'NONE', *, *, #6742, .T. ) ;
#18382 = CONICAL_SURFACE ( 'NONE', #8493, 0.08876456692913387014, 0.7853981624999977207 ) ;
#18383 = DIRECTION ( 'NONE',  ( 0.9999368169139951634, 0.01124109335907400205, 0.000000000000000000 ) ) ;
#18384 = CARTESIAN_POINT ( 'NONE',  ( -0.2938622683360632148, 3.598774863079403804E-17, -3.745078740157480546 ) ) ;
#18385 = TOROIDAL_SURFACE ( 'NONE', #15267, 0.1023622047244094474, 0.003937007874015747977 ) ;
#18386 = PRODUCT_DEFINITION_SHAPE ( 'NONE', 'NONE',  #27887 ) ;
#18387 = DIRECTION ( 'NONE',  ( -0.000000000000000000, -0.000000000000000000, -1.000000000000000000 ) ) ;
#18388 = ORIENTED_EDGE ( 'NONE', *, *, #12754, .T. ) ;
#18389 = CARTESIAN_POINT ( 'NONE',  ( 0.000000000000000000, 0.03937007874015747977, 0.000000000000000000 ) ) ;
#18390 = EDGE_LOOP ( 'NONE', ( #7679, #24414, #15984 ) ) ;
#18391 = CARTESIAN_POINT ( 'NONE',  ( -0.02963280468032113146, 0.4527559054764770385, -1.934055118110236338 ) ) ;
#18392 = CARTESIAN_POINT ( 'NONE',  ( 0.0006345105826664493992, 0.4803145415259079121, 0.2362204724409449896 ) ) ;
#18393 = DIRECTION ( 'NONE',  ( -0.6427876096865393629, 0.7660444431189780135, 0.000000000000000000 ) ) ;
#18394 = CARTESIAN_POINT ( 'NONE',  ( -0.1870078740157480324, 0.000000000000000000, 0.000000000000000000 ) ) ;
#18395 = CIRCLE ( 'NONE', #8935, 0.5393700787401575214 ) ;
#18396 = CARTESIAN_POINT ( 'NONE',  ( -0.6456692913385827515, 0.000000000000000000, -0.01377952755905511792 ) ) ;
#18397 = FACE_OUTER_BOUND ( 'NONE', #6502, .T. ) ;
#18398 = DIRECTION ( 'NONE',  ( 0.000000000000000000, 1.000000000000000000, 0.000000000000000000 ) ) ;
#18399 = ORIENTED_EDGE ( 'NONE', *, *, #8794, .F. ) ;
#18400 = CARTESIAN_POINT ( 'NONE',  ( 0.000000000000000000, 0.000000000000000000, 0.1377952755905511584 ) ) ;
#18401 = DIRECTION ( 'NONE',  ( 0.2225209339563138933, -0.9749279121818237304, 0.000000000000000000 ) ) ;
#18402 = CARTESIAN_POINT ( 'NONE',  ( 0.2693761163850450502, -0.2361997806693590662, -3.115157480314961091 ) ) ;
#18403 = B_SPLINE_CURVE_WITH_KNOTS ( 'NONE', 3,
 ( #22607, #5228, #8167, #13850, #10263, #3227 ),
 .UNSPECIFIED., .F., .F.,
 ( 4, 2, 4 ),
 ( 0.5000000000000000000, 0.7500000000000002220, 1.000000000000000000 ),
 .UNSPECIFIED. ) ;
#18404 = CIRCLE ( 'NONE', #27471, 0.6212598425196850238 ) ;
#18405 = ORIENTED_EDGE ( 'NONE', *, *, #13013, .T. ) ;
#18406 = EDGE_CURVE ( 'NONE', #19493, #720, #16907, .T. ) ;
#18407 = CARTESIAN_POINT ( 'NONE',  ( -0.2006393256663633884, 0.4069519308876736741, -1.934055118110236338 ) ) ;
#18408 = AXIS2_PLACEMENT_3D ( 'NONE', #11973, #25106, #14390 ) ;
#18409 = STYLED_ITEM ( 'NONE', ( #8526 ), #3447 ) ;
#18410 = VERTEX_POINT ( 'NONE', #25519 ) ;
#18411 = ORIENTED_EDGE ( 'NONE', *, *, #20059, .T. ) ;
#18412 = ADVANCED_FACE ( 'NONE', ( #11330 ), #19946, .T. ) ;
#18413 = AXIS2_PLACEMENT_3D ( 'NONE', #436, #16335, #5459 ) ;
#18414 = CARTESIAN_POINT ( 'NONE',  ( -0.3681444341728476455, -0.9492712497839211894, -0.4325618785000000521 ) ) ;
#18415 = CARTESIAN_POINT ( 'NONE',  ( 0.6055690743987126590, 0.5162970762339605946, 0.000000000000000000 ) ) ;
#18416 = CARTESIAN_POINT ( 'NONE',  ( -0.2355331214654133032, 0.4777261797697266998, 1.747047244094488194 ) ) ;
#18417 = EDGE_LOOP ( 'NONE', ( #13145, #2726, #16903, #10478, #8262, #4168, #18827, #22587 ) ) ;
#18418 = ( NAMED_UNIT ( * ) PLANE_ANGLE_UNIT ( ) SI_UNIT ( $, .RADIAN. ) ) ;
#18419 = ORIENTED_EDGE ( 'NONE', *, *, #4573, .T. ) ;
#18420 = CARTESIAN_POINT ( 'NONE',  ( -0.04928467685643870416, 0.3740848232703742893, -3.100567304031763172 ) ) ;
#18421 = DIRECTION ( 'NONE',  ( 0.000000000000000000, 0.000000000000000000, 1.000000000000000000 ) ) ;
#18422 = CARTESIAN_POINT ( 'NONE',  ( -0.2362204724409449064, -0.4724409448818898127, 0.6874452634183660926 ) ) ;
#18423 = AXIS2_PLACEMENT_3D ( 'NONE', #22063, #8696, #17315 ) ;
#18424 = ORIENTED_EDGE ( 'NONE', *, *, #16393, .F. ) ;
#18425 = CYLINDRICAL_SURFACE ( 'NONE', #18413, 2.066929133858267598 ) ;
#18426 = FACE_OUTER_BOUND ( 'NONE', #23201, .T. ) ;
#18427 = TOROIDAL_SURFACE ( 'NONE', #22958, 0.3872945158171015589, 0.01377952755905511792 ) ;
#18428 = ORIENTED_EDGE ( 'NONE', *, *, #12146, .T. ) ;
#18429 = CARTESIAN_POINT ( 'NONE',  ( 0.4417361510194462992, 0.05819755867304002989, -1.934055118110236338 ) ) ;
#18430 = SPHERICAL_SURFACE ( 'NONE', #12349, 0.07677362204724409722 ) ;
#18431 = FACE_OUTER_BOUND ( 'NONE', #9027, .T. ) ;
#18432 = CARTESIAN_POINT ( 'NONE',  ( 0.1791601451668921319, 0.3102476824511487541, -3.115157480314960647 ) ) ;
#18433 = CARTESIAN_POINT ( 'NONE',  ( -0.2775852647713620280, -0.4816145447621894560, 0.9202755905511813550 ) ) ;
#18434 = STYLED_ITEM ( 'NONE', ( #17808 ), #21369 ) ;
#18435 = FACE_OUTER_BOUND ( 'NONE', #11649, .T. ) ;
#18436 = CARTESIAN_POINT ( 'NONE',  ( 0.3722026523000413478, 4.558167867734008572E-17, -0.1033464566929133965 ) ) ;
#18437 = CYLINDRICAL_SURFACE ( 'NONE', #4483, 0.3149606299212598381 ) ;
#18438 = DIRECTION ( 'NONE',  ( 1.000000000000000000, 0.000000000000000000, 0.000000000000000000 ) ) ;
#18439 = FACE_OUTER_BOUND ( 'NONE', #11317, .T. ) ;
#18440 = CARTESIAN_POINT ( 'NONE',  ( -0.09842519685039370636, 0.2165354330708661457, -3.272637795275590733 ) ) ;
#18441 = CARTESIAN_POINT ( 'NONE',  ( -0.4527559055118110520, 0.6889763779527560139, 0.000000000000000000 ) ) ;
#18442 = EDGE_CURVE ( 'NONE', #15836, #1934, #2198, .T. ) ;
#18443 = AXIS2_PLACEMENT_3D ( 'NONE', #5782, #7894, #3206 ) ;
#18444 = ORIENTED_EDGE ( 'NONE', *, *, #33, .F. ) ;
#18445 = DIRECTION ( 'NONE',  ( 0.000000000000000000, 0.000000000000000000, 1.000000000000000000 ) ) ;
#18446 = FACE_OUTER_BOUND ( 'NONE', #17769, .T. ) ;
#18447 = AXIS2_PLACEMENT_3D ( 'NONE', #6800, #69, #15297 ) ;
#18448 = DIRECTION ( 'NONE',  ( 1.000000000000000000, 0.000000000000000000, 0.000000000000000000 ) ) ;
#18449 = EDGE_CURVE ( 'NONE', #5423, #1454, #14811, .T. ) ;
#18450 = VECTOR ( 'NONE', #24105, 39.37007874015748143 ) ;
#18451 = CARTESIAN_POINT ( 'NONE',  ( -0.03478633594543723007, 0.5314960629921260393, 1.747047244094488194 ) ) ;
#18452 = FACE_OUTER_BOUND ( 'NONE', #6398, .T. ) ;
#18453 = CARTESIAN_POINT ( 'NONE',  ( -0.3855916753051542023, -0.3382184156732014890, 1.766732283464566899 ) ) ;
#18454 = ORIENTED_EDGE ( 'NONE', *, *, #2432, .F. ) ;
#18455 = ORIENTED_EDGE ( 'NONE', *, *, #1001, .T. ) ;
#18456 = CARTESIAN_POINT ( 'NONE',  ( 0.1580799066051610802, -0.4326553680327476781, 0.1639447408217406810 ) ) ;
#18457 = ORIENTED_EDGE ( 'NONE', *, *, #16753, .F. ) ;
#18458 = DIRECTION ( 'NONE',  ( 0.000000000000000000, 0.000000000000000000, -1.000000000000000000 ) ) ;
#18459 = DIRECTION ( 'NONE',  ( 0.000000000000000000, 1.000000000000000000, 0.000000000000000000 ) ) ;
#18460 = DIRECTION ( 'NONE',  ( 0.000000000000000000, 1.000000000000000000, 0.000000000000000000 ) ) ;
#18461 = ORIENTED_EDGE ( 'NONE', *, *, #556, .F. ) ;
#18462 = VERTEX_POINT ( 'NONE', #4051 ) ;
#18463 = CARTESIAN_POINT ( 'NONE',  ( 0.06441834428467232976, 0.4889536969035311875, -1.569881889763779625 ) ) ;
#18464 = CARTESIAN_POINT ( 'NONE',  ( -0.09842519685039370636, -1.570035826771653483E-17, -0.09092130223458683158 ) ) ;
#18465 = ORIENTED_EDGE ( 'NONE', *, *, #18731, .T. ) ;
#18466 = EDGE_LOOP ( 'NONE', ( #8355, #6647, #4243, #5808 ) ) ;
#18467 = ORIENTED_EDGE ( 'NONE', *, *, #22413, .F. ) ;
#18468 = ORIENTED_EDGE ( 'NONE', *, *, #22982, .T. ) ;
#18469 = AXIS2_PLACEMENT_3D ( 'NONE', #16572, #18677, #6273 ) ;
#18470 = EDGE_CURVE ( 'NONE', #16095, #14891, #12587, .T. ) ;
#18471 = DIRECTION ( 'NONE',  ( 1.000000000000000000, 0.000000000000000000, 0.000000000000000000 ) ) ;
#18472 = DIRECTION ( 'NONE',  ( 0.000000000000000000, 1.000000000000000000, 0.000000000000000000 ) ) ;
#18473 = PLANE ( 'NONE',  #6877 ) ;
#18474 = DIRECTION ( 'NONE',  ( 0.000000000000000000, 0.000000000000000000, -1.000000000000000000 ) ) ;
#18475 = VERTEX_POINT ( 'NONE', #13439 ) ;
#18476 = EDGE_CURVE ( 'NONE', #23841, #14598, #21625, .T. ) ;
#18477 = AXIS2_PLACEMENT_3D ( 'NONE', #14591, #3525, #12152 ) ;
#18478 = VERTEX_POINT ( 'NONE', #27783 ) ;
#18479 = CARTESIAN_POINT ( 'NONE',  ( -0.4165721057576322606, 0.3313508221749649763, 0.3401574803149606252 ) ) ;
#18480 = EDGE_CURVE ( 'NONE', #8098, #730, #19795, .T. ) ;
#18481 = ORIENTED_EDGE ( 'NONE', *, *, #18104, .F. ) ;
#18482 = DIRECTION ( 'NONE',  ( 1.000000000000000000, 0.000000000000000000, 0.000000000000000000 ) ) ;
#18483 = PLANE ( 'NONE',  #16879 ) ;
#18484 = CARTESIAN_POINT ( 'NONE',  ( -0.6280286859446104764, -0.1014897488084370580, 0.2322205965604635103 ) ) ;
#18485 = CARTESIAN_POINT ( 'NONE',  ( 0.3937007874015748254, 0.000000000000000000, 0.3425196850393700809 ) ) ;
#18486 = CARTESIAN_POINT ( 'NONE',  ( -0.3751294191746890050, 0.2999672986753444404, 0.2194422276354875134 ) ) ;
#18487 = CIRCLE ( 'NONE', #19855, 0.5893189861902062843 ) ;
#18488 = AXIS2_PLACEMENT_3D ( 'NONE', #3215, #2938, #988 ) ;
#18489 = ORIENTED_EDGE ( 'NONE', *, *, #14386, .F. ) ;
#18490 = CARTESIAN_POINT ( 'NONE',  ( 0.2973550541877014175, 0.3552623538112074097, 0.1494804571810765259 ) ) ;
#18491 = VERTEX_POINT ( 'NONE', #9193 ) ;
#18492 = EDGE_CURVE ( 'NONE', #5345, #1951, #15749, .T. ) ;
#18493 = ORIENTED_EDGE ( 'NONE', *, *, #676, .T. ) ;
#18494 = DIRECTION ( 'NONE',  ( 0.000000000000000000, 1.000000000000000000, 0.000000000000000000 ) ) ;
#18495 = FACE_OUTER_BOUND ( 'NONE', #21198, .T. ) ;
#18496 = ORIENTED_EDGE ( 'NONE', *, *, #6857, .F. ) ;
#18497 = CARTESIAN_POINT ( 'NONE',  ( -0.3070866141732283561, 3.760726391082423050E-17, 0.01181102362204724393 ) ) ;
#18498 = ORIENTED_EDGE ( 'NONE', *, *, #1889, .F. ) ;
#18499 = LENGTH_MEASURE_WITH_UNIT ( LENGTH_MEASURE( 0.02539999999999999897 ), #23197 ) ;
#18500 = DIRECTION ( 'NONE',  ( -1.000000000000000000, 0.000000000000000000, 0.000000000000000000 ) ) ;
#18501 = DIRECTION ( 'NONE',  ( 0.000000000000000000, -1.000000000000000000, 0.000000000000000000 ) ) ;
#18502 = EDGE_CURVE ( 'NONE', #27673, #22433, #13046, .T. ) ;
#18503 = AXIS2_PLACEMENT_3D ( 'NONE', #159, #4497, #8730 ) ;
#18504 = DIRECTION ( 'NONE',  ( 0.000000000000000000, 1.000000000000000000, 0.000000000000000000 ) ) ;
#18505 = DIRECTION ( 'NONE',  ( -0.9659258263664933786, 0.2588190448135661570, 3.169619147893090844E-17 ) ) ;
#18506 = EDGE_CURVE ( 'NONE', #7118, #1047, #17230, .T. ) ;
#18507 = ORIENTED_EDGE ( 'NONE', *, *, #4066, .F. ) ;
#18508 = CARTESIAN_POINT ( 'NONE',  ( 0.02190250779246040100, 0.3346456692913385988, 1.973425196850393970 ) ) ;
#18509 = CARTESIAN_POINT ( 'NONE',  ( -0.4932821129636645874, 0.08637579872942342807, 0.2574803149606298969 ) ) ;
#18510 = CARTESIAN_POINT ( 'NONE',  ( 0.3121994997578124154, -0.4069448477569433953, -1.550196850393700920 ) ) ;
#18511 = EDGE_CURVE ( 'NONE', #3709, #17997, #20580, .T. ) ;
#18512 = CARTESIAN_POINT ( 'NONE',  ( -0.5511811023622046335, 0.07214943758244282690, 0.9202755905511811330 ) ) ;
#18513 = AXIS2_PLACEMENT_3D ( 'NONE', #2744, #19307, #19725 ) ;
#18514 = CARTESIAN_POINT ( 'NONE',  ( -0.4152525734086447429, -0.3642352168757386210, 0.9202755905511811330 ) ) ;
#18515 = DIRECTION ( 'NONE',  ( 0.000000000000000000, 0.000000000000000000, -1.000000000000000000 ) ) ;
#18516 = CARTESIAN_POINT ( 'NONE',  ( -0.1771653543307086520, -5.663984251968503442E-18, -0.1476377952755905387 ) ) ;
#18517 = ORIENTED_EDGE ( 'NONE', *, *, #12576, .F. ) ;
#18518 = CARTESIAN_POINT ( 'NONE',  ( 0.5981657849660177995, -0.2403521948818897747, -0.4163022132461299263 ) ) ;
#18519 = ADVANCED_FACE ( 'NONE', ( #5054 ), #2525, .T. ) ;
#18520 = CARTESIAN_POINT ( 'NONE',  ( 0.3765118517642103146, -0.04928528614549727849, -3.100567304031763172 ) ) ;
#18521 = ORIENTED_EDGE ( 'NONE', *, *, #17482, .T. ) ;
#18522 = CARTESIAN_POINT ( 'NONE',  ( 0.4245040230928834313, 0.7010584879324154306, -0.6327280771288582573 ) ) ;
#18523 = EDGE_CURVE ( 'NONE', #10848, #7459, #13470, .T. ) ;
#18524 = ORIENTED_EDGE ( 'NONE', *, *, #12030, .T. ) ;
#18525 = VECTOR ( 'NONE', #19577, 39.37007874015748143 ) ;
#18526 = DIRECTION ( 'NONE',  ( 1.000000000000000000, 0.000000000000000000, 0.000000000000000000 ) ) ;
#18527 = FACE_OUTER_BOUND ( 'NONE', #10006, .T. ) ;
#18528 = EDGE_LOOP ( 'NONE', ( #7512, #9526, #19170, #8597, #18755, #3389, #5571, #11108, #413, #10583, #15045, #4068, #17937, #15937, #12844, #5869 ) ) ;
#18529 = DIRECTION ( 'NONE',  ( 1.000000000000000000, 0.000000000000000000, 0.000000000000000000 ) ) ;
#18530 = CARTESIAN_POINT ( 'NONE',  ( 0.2019525613798653640, -0.7328932975451569742, 7.384975690285532084E-17 ) ) ;
#18531 = ORIENTED_EDGE ( 'NONE', *, *, #15498, .T. ) ;
#18532 = ORIENTED_EDGE ( 'NONE', *, *, #17744, .F. ) ;
#18533 = VECTOR ( 'NONE', #10668, 39.37007874015748143 ) ;
#18534 = TOROIDAL_SURFACE ( 'NONE', #15435, 0.1476377952755905387, 0.01968503937007873988 ) ;
#18535 = CARTESIAN_POINT ( 'NONE',  ( -0.08530183727034115759, -0.03937007874015747977, 0.06819097667594049839 ) ) ;
#18536 = CARTESIAN_POINT ( 'NONE',  ( 0.000000000000000000, 0.000000000000000000, 0.1771653543307086520 ) ) ;
#18537 = CYLINDRICAL_SURFACE ( 'NONE', #1980, 0.1082677165354330312 ) ;
#18538 = AXIS2_PLACEMENT_3D ( 'NONE', #16689, #27711, #12298 ) ;
#18539 = FACE_OUTER_BOUND ( 'NONE', #7154, .T. ) ;
#18540 = DIRECTION ( 'NONE',  ( -1.000000000000000000, 1.224646799147353454E-16, 0.000000000000000000 ) ) ;
#18541 = DIRECTION ( 'NONE',  ( 1.000000000000000000, 0.000000000000000000, 0.000000000000000000 ) ) ;
#18542 = ORIENTED_EDGE ( 'NONE', *, *, #15878, .F. ) ;
#18543 = DIRECTION ( 'NONE',  ( -0.2036417511401760472, -0.4895227362422912565, 0.8478782506317888989 ) ) ;
#18544 = DIRECTION ( 'NONE',  ( 1.000000000000000000, 0.000000000000000000, 0.000000000000000000 ) ) ;
#18545 = EDGE_CURVE ( 'NONE', #24440, #3752, #9810, .T. ) ;
#18546 = DIRECTION ( 'NONE',  ( -0.7071067818211350664, 0.000000000000000000, -0.7071067805519599681 ) ) ;
#18547 = CARTESIAN_POINT ( 'NONE',  ( -0.04673558830912487999, -0.3552036222398666232, -3.115157480314960647 ) ) ;
#18548 = EDGE_CURVE ( 'NONE', #26883, #10706, #22270, .T. ) ;
#18549 = ORIENTED_EDGE ( 'NONE', *, *, #16614, .T. ) ;
#18550 = CARTESIAN_POINT ( 'NONE',  ( -0.02909913904662018644, 0.4446020952038907681, -1.934055118110236338 ) ) ;
#18551 = EDGE_CURVE ( 'NONE', #12714, #6891, #9150, .T. ) ;
#18552 = ( GEOMETRIC_REPRESENTATION_CONTEXT ( 3 ) GLOBAL_UNCERTAINTY_ASSIGNED_CONTEXT ( ( #5368 ) ) GLOBAL_UNIT_ASSIGNED_CONTEXT ( ( #4839, #15858, #22362 ) ) REPRESENTATION_CONTEXT ( 'NONE', 'WORKASPACE' ) ) ;
#18553 = ORIENTED_EDGE ( 'NONE', *, *, #13053, .T. ) ;
#18554 = CARTESIAN_POINT ( 'NONE',  ( -0.4101012214746874163, -0.7973509628734607446, -0.2476620753154787635 ) ) ;
#18555 = DIRECTION ( 'NONE',  ( 0.000000000000000000, -1.000000000000000000, 0.000000000000000000 ) ) ;
#18556 = CARTESIAN_POINT ( 'NONE',  ( -0.4225965726692976765, -0.3242071728275119913, 1.747047244094488194 ) ) ;
#18557 = ORIENTED_EDGE ( 'NONE', *, *, #20021, .T. ) ;
#18558 = EDGE_LOOP ( 'NONE', ( #15222, #21545, #15220, #4058 ) ) ;
#18559 = DIRECTION ( 'NONE',  ( 0.000000000000000000, 0.000000000000000000, 1.000000000000000000 ) ) ;
#18560 = CARTESIAN_POINT ( 'NONE',  ( 0.2228021814271965440, -0.4641672719422391125, 0.1473214333490711070 ) ) ;
#18561 = B_SPLINE_SURFACE_WITH_KNOTS ( 'NONE', 3, 3, ( 
 ( #2142, #12873, #25928, #21418, #8556, #2055 ),
 ( #119, #17176, #10667, #6720, #19288, #25790 ),
 ( #20888, #23022, #8692, #6646, #6438, #10952 ),
 ( #8825, #10529, #15358, #4456, #23950, #23685 ) ),
 .UNSPECIFIED., .F., .F., .F.,
 ( 4, 4 ),
 ( 4, 1, 1, 4 ),
 ( -0.1429447353023790002, 0.1429447353023790002 ),
 ( -0.2617993877991500185, -0.03739991254273600241, 0.1121997376282070080, 0.2617993877991500185 ),
 .UNSPECIFIED. ) ;
#18562 = FACE_OUTER_BOUND ( 'NONE', #14739, .T. ) ;
#18563 = ORIENTED_EDGE ( 'NONE', *, *, #608, .T. ) ;
#18564 = CARTESIAN_POINT ( 'NONE',  ( 0.1294857240059045234, -0.3542416573274181357, 0.1992125984251968684 ) ) ;
#18565 = DIRECTION ( 'NONE',  ( 0.000000000000000000, 0.000000000000000000, -1.000000000000000000 ) ) ;
#18566 = EDGE_LOOP ( 'NONE', ( #5711, #16748, #19162, #135, #20108, #8705, #10158, #17981, #10162, #26934, #4409, #1352, #17518, #26424 ) ) ;
#18567 = CARTESIAN_POINT ( 'NONE',  ( -0.05819755867304135522, -0.4417361510194244278, -1.934055118110236338 ) ) ;
#18568 = ORIENTED_EDGE ( 'NONE', *, *, #25423, .F. ) ;
#18569 = ORIENTED_EDGE ( 'NONE', *, *, #19919, .T. ) ;
#18570 = CARTESIAN_POINT ( 'NONE',  ( 0.5925575908939920700, -0.4537419570391968415, 5.556736220472441090E-17 ) ) ;
#18571 = FACE_OUTER_BOUND ( 'NONE', #12329, .T. ) ;
#18572 = AXIS2_PLACEMENT_3D ( 'NONE', #24894, #12574, #19060 ) ;
#18573 = FACE_OUTER_BOUND ( 'NONE', #23413, .T. ) ;
#18574 = CARTESIAN_POINT ( 'NONE',  ( 0.1791601451668926592, -0.3102476824511484210, -3.115157480314960647 ) ) ;
#18575 = DIRECTION ( 'NONE',  ( -0.6234898018587338164, -0.7818314824680293595, 0.000000000000000000 ) ) ;
#18576 = CARTESIAN_POINT ( 'NONE',  ( -0.2924088307484721261, 0.1685339107540411718, 1.973425196850393526 ) ) ;
#18577 = CARTESIAN_POINT ( 'NONE',  ( 0.000000000000000000, 0.000000000000000000, 2.426181102355854158 ) ) ;
#18578 = AXIS2_PLACEMENT_3D ( 'NONE', #22986, #14666, #10242 ) ;
#18579 = DIRECTION ( 'NONE',  ( 0.000000000000000000, 0.000000000000000000, -1.000000000000000000 ) ) ;
#18580 = CARTESIAN_POINT ( 'NONE',  ( -0.7874015748031496509, 0.9829781505553011334, -0.2190361720152886049 ) ) ;
#18581 = CARTESIAN_POINT ( 'NONE',  ( -0.4055118110236220486, -0.4724409448818898127, -0.8182917201112815953 ) ) ;
#18582 = CARTESIAN_POINT ( 'NONE',  ( 0.5190862322091315262, -0.1177929122753177127, 0.3401574803149606252 ) ) ;
#18583 = AXIS2_PLACEMENT_3D ( 'NONE', #20947, #14624, #16999 ) ;
#18584 = ORIENTED_EDGE ( 'NONE', *, *, #7364, .T. ) ;
#18585 = CARTESIAN_POINT ( 'NONE',  ( -0.4538399017594920148, 0.3483099419441555988, 0.9399606299212600602 ) ) ;
#18586 = CARTESIAN_POINT ( 'NONE',  ( 0.5118110236220472231, 0.000000000000000000, 1.747047244094488194 ) ) ;
#18587 = AXIS2_PLACEMENT_3D ( 'NONE', #10599, #19223, #27855 ) ;
#18588 = CARTESIAN_POINT ( 'NONE',  ( -0.2362204724409449064, -0.4724409448818898127, 0.8182917201112794858 ) ) ;
#18589 = VERTEX_POINT ( 'NONE', #17374 ) ;
#18590 = FACE_OUTER_BOUND ( 'NONE', #9151, .T. ) ;
#18591 = DIRECTION ( 'NONE',  ( -0.3420201433256691570, -0.9396926207859082059, 0.000000000000000000 ) ) ;
#18592 = CARTESIAN_POINT ( 'NONE',  ( 0.03349795313264414959, -0.5118110236220472231, 1.747047244094488194 ) ) ;
#18593 = DIRECTION ( 'NONE',  ( -1.000000000000000000, 0.000000000000000000, 0.000000000000000000 ) ) ;
#18594 = CARTESIAN_POINT ( 'NONE',  ( 0.1649135259616801574, 0.4856708409200201637, 1.747047244094488194 ) ) ;
#18595 = EDGE_LOOP ( 'NONE', ( #18964, #13401, #3063, #25367, #338 ) ) ;
#18596 = CIRCLE ( 'NONE', #3262, 0.1181010187939084827 ) ;
#18597 = VERTEX_POINT ( 'NONE', #24407 ) ;
#18598 = CARTESIAN_POINT ( 'NONE',  ( 0.000000000000000000, 0.000000000000000000, 0.1377952755905511584 ) ) ;
#18599 = VERTEX_POINT ( 'NONE', #4642 ) ;
#18600 = CARTESIAN_POINT ( 'NONE',  ( -6.518592411209533944E-17, -0.5322834645669292097, 0.1322834645669291320 ) ) ;
#18601 = CARTESIAN_POINT ( 'NONE',  ( -0.5905511811023621549, -0.4526313213353566622, -0.9943460912301791410 ) ) ;
#18602 = ( NAMED_UNIT ( * ) SI_UNIT ( $, .STERADIAN. ) SOLID_ANGLE_UNIT ( ) ) ;
#18603 = EDGE_CURVE ( 'NONE', #18589, #10030, #25990, .T. ) ;
#18604 = CARTESIAN_POINT ( 'NONE',  ( 0.1504778549387067454, -0.4839706879307174581, 0.03773480285810273255 ) ) ;
#18605 = CARTESIAN_POINT ( 'NONE',  ( 0.3346456692913385988, 0.02190250779246873461, 1.973425196850393970 ) ) ;
#18606 = VERTEX_POINT ( 'NONE', #7051 ) ;
#18607 = ADVANCED_FACE ( 'NONE', ( #6781 ), #13063, .F. ) ;
#18608 = ORIENTED_EDGE ( 'NONE', *, *, #16491, .T. ) ;
#18609 = CARTESIAN_POINT ( 'NONE',  ( -0.1585706980422471879, 0.4669911931914806913, -1.569881889763779625 ) ) ;
#18610 = ORIENTED_EDGE ( 'NONE', *, *, #17818, .T. ) ;
#18611 = VERTEX_POINT ( 'NONE', #9020 ) ;
#18612 = EDGE_CURVE ( 'NONE', #25825, #11779, #20256, .T. ) ;
#18613 = TOROIDAL_SURFACE ( 'NONE', #24449, 0.6102362204724409711, 0.1299212598425196763 ) ;
#18614 = VECTOR ( 'NONE', #5437, 39.37007874015748143 ) ;
#18615 = EDGE_CURVE ( 'NONE', #2791, #5588, #9432, .T. ) ;
#18616 = CARTESIAN_POINT ( 'NONE',  ( -0.3726024258163779246, 4.563063681305663643E-17, -3.115157480314960647 ) ) ;
#18617 = DIRECTION ( 'NONE',  ( -0.000000000000000000, 1.000000000000000000, -0.000000000000000000 ) ) ;
#18618 = CARTESIAN_POINT ( 'NONE',  ( -0.3480868068226445344, 0.1863314354528550765, 0.2260787492974006274 ) ) ;
#18619 = ORIENTED_EDGE ( 'NONE', *, *, #169, .F. ) ;
#18620 = CARTESIAN_POINT ( 'NONE',  ( 0.09590060490395689585, 0.1136516277932334562, 0.1968503937007874127 ) ) ;
#18621 = ( REPRESENTATION_RELATIONSHIP ('NONE','NONE', #12434, #16232 ) REPRESENTATION_RELATIONSHIP_WITH_TRANSFORMATION ( #27119 )SHAPE_REPRESENTATION_RELATIONSHIP( ) ) ;
#18622 = UNCERTAINTY_MEASURE_WITH_UNIT (LENGTH_MEASURE( 1.000000000000000082E-05 ), #8487, 'distance_accuracy_value', 'NONE') ;
#18623 = DIRECTION ( 'NONE',  ( 0.000000000000000000, 1.000000000000000000, 0.000000000000000000 ) ) ;
#18624 = CARTESIAN_POINT ( 'NONE',  ( 0.2118615749922956593, -0.5840192333899354438, 0.09685039370078740717 ) ) ;
#18625 = CARTESIAN_POINT ( 'NONE',  ( -0.5950316419613312924, -0.2176117105159648402, 0.2177171427811122051 ) ) ;
#18626 = PLANE ( 'NONE',  #23218 ) ;
#18627 = DIRECTION ( 'NONE',  ( -1.000000000000000000, 0.000000000000000000, 0.000000000000000000 ) ) ;
#18628 = VECTOR ( 'NONE', #13101, 39.37007874015748143 ) ;
#18629 = AXIS2_PLACEMENT_3D ( 'NONE', #4687, #15044, #94 ) ;
#18630 = ORIENTED_EDGE ( 'NONE', *, *, #22166, .T. ) ;
#18631 = VERTEX_POINT ( 'NONE', #24004 ) ;
#18632 = CIRCLE ( 'NONE', #22250, 0.1299232283464567261 ) ;
#18633 = ( NAMED_UNIT ( * ) PLANE_ANGLE_UNIT ( ) SI_UNIT ( $, .RADIAN. ) ) ;
#18634 = ORIENTED_EDGE ( 'NONE', *, *, #17223, .F. ) ;
#18635 = ADVANCED_FACE ( 'NONE', ( #13268 ), #26258, .T. ) ;
#18636 = CARTESIAN_POINT ( 'NONE',  ( 0.2952755905264887182, 0.000000000000000000, 0.9055118110027171596 ) ) ;
#18637 = EDGE_CURVE ( 'NONE', #20701, #20032, #15351, .T. ) ;
#18638 = AXIS2_PLACEMENT_3D ( 'NONE', #25276, #7772, #14126 ) ;
#18639 = CARTESIAN_POINT ( 'NONE',  ( 1.692913385826771533, 0.07874015748031491790, 0.1181102362204723144 ) ) ;
#18640 = ORIENTED_EDGE ( 'NONE', *, *, #8834, .T. ) ;
#18641 = EDGE_CURVE ( 'NONE', #15836, #5312, #889, .T. ) ;
#18642 = ORIENTED_EDGE ( 'NONE', *, *, #11193, .T. ) ;
#18643 = CARTESIAN_POINT ( 'NONE',  ( -0.5905511811023621549, 0.000000000000000000, 0.000000000000000000 ) ) ;
#18644 = ADVANCED_FACE ( 'NONE', ( #26812 ), #3491, .F. ) ;
#18645 = DIRECTION ( 'NONE',  ( 1.000000000000000000, 0.000000000000000000, 0.000000000000000000 ) ) ;
#18646 = CARTESIAN_POINT ( 'NONE',  ( -0.1968503937007874127, -0.4724409448818898127, -0.9265594366467145848 ) ) ;
#18647 = AXIS2_PLACEMENT_3D ( 'NONE', #5107, #24599, #13731 ) ;
#18648 = CARTESIAN_POINT ( 'NONE',  ( -0.06889763779527552368, 0.000000000000000000, -0.2834645669291338543 ) ) ;
#18649 = CARTESIAN_POINT ( 'NONE',  ( -0.03532354024591771724, 0.000000000000000000, 0.000000000000000000 ) ) ;
#18650 = ORIENTED_EDGE ( 'NONE', *, *, #22693, .T. ) ;
#18651 = CARTESIAN_POINT ( 'NONE',  ( 0.3175540113612324578, -0.1078280746903944320, 1.973425196850393970 ) ) ;
#18652 = CARTESIAN_POINT ( 'NONE',  ( 0.4069448477569526101, -0.3121994997578271813, -1.550196850393700920 ) ) ;
#18653 = ADVANCED_FACE ( 'NONE', ( #25118 ), #1767, .F. ) ;
#18654 = FACE_OUTER_BOUND ( 'NONE', #14174, .T. ) ;
#18655 = VECTOR ( 'NONE', #5838, 39.37007874015748143 ) ;
#18656 = CARTESIAN_POINT ( 'NONE',  ( 0.2442565704126313797, -0.4954197419817796266, 0.9399606299212598381 ) ) ;
#18657 = CARTESIAN_POINT ( 'NONE',  ( 0.2428345617565153547, 0.2885915454824177218, 0.1992125984251968684 ) ) ;
#18658 = AXIS2_PLACEMENT_3D ( 'NONE', #12885, #15032, #19389 ) ;
#18659 = CARTESIAN_POINT ( 'NONE',  ( -4.618943439303797186E-17, -0.3771653543307086909, 0.1992125984251968684 ) ) ;
#18660 = CARTESIAN_POINT ( 'NONE',  ( 0.5525004126151165096, 0.09742072959660433296, 0.07676968503937006694 ) ) ;
#18661 = DIRECTION ( 'NONE',  ( 1.000000000000000000, 0.000000000000000000, 0.000000000000000000 ) ) ;
#18662 = CARTESIAN_POINT ( 'NONE',  ( 0.03965503742771028101, 0.1968503937007873850, -3.203835717288081142 ) ) ;
#18663 = TOROIDAL_SURFACE ( 'NONE', #18192, 0.6102362204724409711, 0.1299212598425196763 ) ;
#18664 = VERTEX_POINT ( 'NONE', #27248 ) ;
#18665 = DIRECTION ( 'NONE',  ( 0.9996775636078711891, 0.000000000000000000, 0.02539229841961800765 ) ) ;
#18666 = CARTESIAN_POINT ( 'NONE',  ( 0.4055118110236220486, 0.000000000000000000, 0.3425196850393700809 ) ) ;
#18667 = CARTESIAN_POINT ( 'NONE',  ( 0.4010740433761567081, 4.911740434416970370E-17, -0.2342519685039370358 ) ) ;
#18668 = CYLINDRICAL_SURFACE ( 'NONE', #25379, 0.5322834645669292097 ) ;
#18669 = EDGE_CURVE ( 'NONE', #17886, #16657, #3564, .T. ) ;
#18670 = ORIENTED_EDGE ( 'NONE', *, *, #16205, .F. ) ;
#18671 = DIRECTION ( 'NONE',  ( 0.000000000000000000, 0.000000000000000000, 1.000000000000000000 ) ) ;
#18672 = ORIENTED_EDGE ( 'NONE', *, *, #18669, .T. ) ;
#18673 = AXIS2_PLACEMENT_3D ( 'NONE', #17631, #22018, #13390 ) ;
#18674 = CARTESIAN_POINT ( 'NONE',  ( 0.000000000000000000, 0.9055118110236217710, -0.2952755905511805223 ) ) ;
#18675 = DIRECTION ( 'NONE',  ( -1.000000000000000000, 0.000000000000000000, 0.000000000000000000 ) ) ;
#18676 = CIRCLE ( 'NONE', #27729, 0.1751968503937007815 ) ;
#18677 = DIRECTION ( 'NONE',  ( 0.000000000000000000, 0.000000000000000000, -1.000000000000000000 ) ) ;
#18678 = CARTESIAN_POINT ( 'NONE',  ( 0.000000000000000000, 0.000000000000000000, 0.01181102362204724393 ) ) ;
#18679 = CARTESIAN_POINT ( 'NONE',  ( 0.4898768902087983768, -1.879168897637795438E-16, 0.07874015748031495954 ) ) ;
#18680 = EDGE_CURVE ( 'NONE', #13695, #10695, #9891, .T. ) ;
#18681 = EDGE_LOOP ( 'NONE', ( #15388, #3026, #25604, #25749 ) ) ;
#18682 = CARTESIAN_POINT ( 'NONE',  ( 0.000000000000000000, 0.000000000000000000, 0.4488188976377953110 ) ) ;
#18683 = DIRECTION ( 'NONE',  ( -0.7660444431189774583, 0.6427876096865400291, 0.000000000000000000 ) ) ;
#18684 = CARTESIAN_POINT ( 'NONE',  ( 0.1493967478962657525, 0.4798749592428784849, 0.01883130896441918486 ) ) ;
#18685 = ORIENTED_EDGE ( 'NONE', *, *, #14295, .F. ) ;
#18686 = DIRECTION ( 'NONE',  ( -1.000000000000000000, -1.224646799147353454E-16, 0.000000000000000000 ) ) ;
#18687 = CARTESIAN_POINT ( 'NONE',  ( 0.4895462770359960136, 0.6604130065487362478, -0.5726600247964968027 ) ) ;
#18688 = CARTESIAN_POINT ( 'NONE',  ( 0.3707612262533033776, -0.3252100150720387273, -1.569881889763779625 ) ) ;
#18689 = CIRCLE ( 'NONE', #26356, 0.1003956692913385573 ) ;
#18690 = ADVANCED_FACE ( 'NONE', ( #12260 ), #19380, .T. ) ;
#18691 = UNCERTAINTY_MEASURE_WITH_UNIT (LENGTH_MEASURE( 1.000000000000000082E-05 ), #3059, 'distance_accuracy_value', 'NONE') ;
#18692 = VERTEX_POINT ( 'NONE', #1257 ) ;
#18693 = CARTESIAN_POINT ( 'NONE',  ( -0.2712027394948519632, -0.3535065162672669792, -1.934055118110236338 ) ) ;
#18694 = CARTESIAN_POINT ( 'NONE',  ( -0.3979194638820524044, 0.2297883689023302312, -1.928289503579153630 ) ) ;
#18695 = VECTOR ( 'NONE', #19699, 39.37007874015748143 ) ;
#18696 = EDGE_LOOP ( 'NONE', ( #13860, #6468, #1106, #1597, #3025, #23671 ) ) ;
#18697 = ORIENTED_EDGE ( 'NONE', *, *, #4467, .T. ) ;
#18698 = VERTEX_POINT ( 'NONE', #16369 ) ;
#18699 = AXIS2_PLACEMENT_3D ( 'NONE', #24945, #13800, #5173 ) ;
#18700 = CARTESIAN_POINT ( 'NONE',  ( 0.5375739373539409893, 0.4296723508511047229, 0.3401574803149606252 ) ) ;
#18701 = DIRECTION ( 'NONE',  ( 0.000000000000000000, -1.000000000000000000, 0.000000000000000000 ) ) ;
#18702 = CARTESIAN_POINT ( 'NONE',  ( 0.5280699926562892887, 0.06957181182498746452, 1.747047244094488194 ) ) ;
#18703 = ORIENTED_EDGE ( 'NONE', *, *, #21085, .T. ) ;
#18704 = ORIENTED_EDGE ( 'NONE', *, *, #3008, .T. ) ;
#18705 = FILL_AREA_STYLE ('',( #20977 ) ) ;
#18706 = EDGE_LOOP ( 'NONE', ( #12171, #15304, #6241, #12218, #19352 ) ) ;
#18707 = ADVANCED_FACE ( 'NONE', ( #10003 ), #4502, .F. ) ;
#18708 = CARTESIAN_POINT ( 'NONE',  ( 0.3740848232703748444, 0.04928467685643974500, -3.100567304031760507 ) ) ;
#18709 = DIRECTION ( 'NONE',  ( 1.000000000000000000, 0.000000000000000000, 0.000000000000000000 ) ) ;
#18710 = CARTESIAN_POINT ( 'NONE',  ( 0.5925575908939920700, 0.000000000000000000, 0.000000000000000000 ) ) ;
#18711 = EDGE_CURVE ( 'NONE', #6276, #11990, #5380, .T. ) ;
#18712 = AXIS2_PLACEMENT_3D ( 'NONE', #19444, #10543, #14821 ) ;
#18713 = CARTESIAN_POINT ( 'NONE',  ( -0.2161381151963043257, -0.2817310484609166221, 1.953740157480315043 ) ) ;
#18714 = VERTEX_POINT ( 'NONE', #22719 ) ;
#18715 = DIRECTION ( 'NONE',  ( -0.000000000000000000, -1.000000000000000000, -0.000000000000000000 ) ) ;
#18716 = CYLINDRICAL_SURFACE ( 'NONE', #17860, 0.4685039370078740717 ) ;
#18718 = CARTESIAN_POINT ( 'NONE',  ( 0.1480156394741987402, 0.5526079293737075071, 0.9399606299212598381 ) ) ;
#18717 = CARTESIAN_POINT ( 'NONE',  ( -0.3765118517642103702, -0.04928528614549713277, -3.100567304031763172 ) ) ;
#18719 = FACE_OUTER_BOUND ( 'NONE', #17861, .T. ) ;
#18720 = B_SPLINE_CURVE_WITH_KNOTS ( 'NONE', 3,
 ( #22922, #25028, #14170, #5692, #12169, #12462 ),
 .UNSPECIFIED., .F., .F.,
 ( 4, 2, 4 ),
 ( 0.5000000000000000000, 0.7500000000000001110, 1.000000000000000000 ),
 .UNSPECIFIED. ) ;
#18721 = ORIENTED_EDGE ( 'NONE', *, *, #5252, .F. ) ;
#18722 = VERTEX_POINT ( 'NONE', #3345 ) ;
#18723 = FACE_OUTER_BOUND ( 'NONE', #11711, .T. ) ;
#18724 = CIRCLE ( 'NONE', #14724, 0.2395669291338582696 ) ;
#18725 = CARTESIAN_POINT ( 'NONE',  ( -0.1791601451668828893, 0.3102476824511414266, -3.115157480314960647 ) ) ;
#18726 = CIRCLE ( 'NONE', #21457, 0.1771653543307086520 ) ;
#18727 = DIRECTION ( 'NONE',  ( 0.000000000000000000, 1.000000000000000000, 0.000000000000000000 ) ) ;
#18728 = DIRECTION ( 'NONE',  ( 0.000000000000000000, -1.000000000000000000, 0.000000000000000000 ) ) ;
#18729 = DIRECTION ( 'NONE',  ( -1.000000000000000000, 0.000000000000000000, 0.000000000000000000 ) ) ;
#18730 = CARTESIAN_POINT ( 'NONE',  ( -0.2490711204941342405, 0.7655264129003995777, -0.7689379837741201484 ) ) ;
#18731 = EDGE_CURVE ( 'NONE', #7534, #9015, #5416, .T. ) ;
#18732 = FACE_OUTER_BOUND ( 'NONE', #3910, .T. ) ;
#18733 = CARTESIAN_POINT ( 'NONE',  ( 1.197070535079588716, 0.07874015748031491790, -1.197070535079588716 ) ) ;
#18734 = CARTESIAN_POINT ( 'NONE',  ( 0.3543307086614173596, 0.000000000000000000, 1.953740157480315043 ) ) ;
#18735 = AXIS2_PLACEMENT_3D ( 'NONE', #15856, #24460, #7813 ) ;
#18736 = ORIENTED_EDGE ( 'NONE', *, *, #11218, .F. ) ;
#18737 = CARTESIAN_POINT ( 'NONE',  ( 0.3771696032822623446, 0.4301590433674484792, 0.9399606299212601712 ) ) ;
#18738 = CARTESIAN_POINT ( 'NONE',  ( 0.4898768902087983768, 0.000000000000000000, 0.2362204724409449064 ) ) ;
#18739 = DIRECTION ( 'NONE',  ( 0.000000000000000000, 0.000000000000000000, 1.000000000000000000 ) ) ;
#18740 = ORIENTED_EDGE ( 'NONE', *, *, #1889, .T. ) ;
#18741 = CARTESIAN_POINT ( 'NONE',  ( 0.000000000000000000, 0.000000000000000000, -0.4724409448841456749 ) ) ;
#18742 = CARTESIAN_POINT ( 'NONE',  ( 0.4004221243553557907, -0.3512268162760437407, 1.747047244094488194 ) ) ;
#18743 = DIRECTION ( 'NONE',  ( 1.000000000000000000, 0.000000000000000000, 0.000000000000000000 ) ) ;
#18744 = CARTESIAN_POINT ( 'NONE',  ( -0.4954415918530857832, 0.1327036767659614813, 1.766732283464566899 ) ) ;
#18745 = ORIENTED_EDGE ( 'NONE', *, *, #4412, .T. ) ;
#18746 = ORIENTED_EDGE ( 'NONE', *, *, #15288, .F. ) ;
#18747 = CARTESIAN_POINT ( 'NONE',  ( -0.3040421205569480145, 0.7911861580938169825, -0.8381822164908544481 ) ) ;
#18748 = ORIENTED_EDGE ( 'NONE', *, *, #23502, .T. ) ;
#18749 = ADVANCED_FACE ( 'NONE', ( #5495 ), #15769, .F. ) ;
#18750 = VECTOR ( 'NONE', #7477, 39.37007874015748143 ) ;
#18751 = DIRECTION ( 'NONE',  ( 0.000000000000000000, 0.000000000000000000, 1.000000000000000000 ) ) ;
#18752 = EDGE_CURVE ( 'NONE', #11291, #26680, #12608, .T. ) ;
#18753 = CARTESIAN_POINT ( 'NONE',  ( -0.04380447413658894451, -0.3324885138898239778, 1.973425196850393970 ) ) ;
#18754 = ORIENTED_EDGE ( 'NONE', *, *, #17507, .T. ) ;
#18755 = ORIENTED_EDGE ( 'NONE', *, *, #24031, .T. ) ;
#18756 = ORIENTED_EDGE ( 'NONE', *, *, #23935, .F. ) ;
#18757 = CIRCLE ( 'NONE', #21475, 0.05216535433070866590 ) ;
#18758 = VERTEX_POINT ( 'NONE', #7321 ) ;
#18759 = ORIENTED_EDGE ( 'NONE', *, *, #588, .F. ) ;
#18760 = CONTEXT_DEPENDENT_SHAPE_REPRESENTATION ( #24397, #26283 ) ;
#18761 = FACE_OUTER_BOUND ( 'NONE', #21028, .T. ) ;
#18762 = CARTESIAN_POINT ( 'NONE',  ( 0.5382469622846938195, -0.3102483656526054956, 0.09684874924366436433 ) ) ;
#18763 = DIRECTION ( 'NONE',  ( -0.8660254037844390407, -0.4999999999999994449, 0.000000000000000000 ) ) ;
#18764 = ORIENTED_EDGE ( 'NONE', *, *, #765, .T. ) ;
#18765 = CARTESIAN_POINT ( 'NONE',  ( -0.3220512119205936608, 0.3834984712787528061, 0.2574827755769819038 ) ) ;
#18766 = AXIS2_PLACEMENT_3D ( 'NONE', #5086, #27273, #10163 ) ;
#18767 = ADVANCED_BREP_SHAPE_REPRESENTATION ( 'O-Ring 26.5x2.65', ( #12535, #11588 ), #16570 ) ;
#18768 = DIRECTION ( 'NONE',  ( 1.000000000000000000, 0.000000000000000000, 0.000000000000000000 ) ) ;
#18769 = ADVANCED_FACE ( 'NONE', ( #22872, #5633, #27108, #7613, #1120 ), #11841, .T. ) ;
#18770 = FACE_BOUND ( 'NONE', #3662, .T. ) ;
#18771 = CARTESIAN_POINT ( 'NONE',  ( 0.9842519685039370358, 2.925196850393700920, -0.6496062992125984925 ) ) ;
#18772 = AXIS2_PLACEMENT_3D ( 'NONE', #3552, #12182, #1734 ) ;
#18773 = CARTESIAN_POINT ( 'NONE',  ( -0.6020290825756511310, -0.1931961917790488426, 0.2216582221849488499 ) ) ;
#18774 = CARTESIAN_POINT ( 'NONE',  ( -6.132876883919029269E-17, -0.5007874015748031704, 0.04842519685039370358 ) ) ;
#18775 = DIRECTION ( 'NONE',  ( -0.000000000000000000, 0.000000000000000000, -1.000000000000000000 ) ) ;
#18776 = EDGE_LOOP ( 'NONE', ( #18974, #17103, #9811, #6152 ) ) ;
#18777 = ADVANCED_FACE ( 'NONE', ( #22437 ), #5743, .T. ) ;
#18778 = CARTESIAN_POINT ( 'NONE',  ( 0.4442166144915702941, 0.2564158049319635868, -1.550196850393700476 ) ) ;
#18779 = ORIENTED_EDGE ( 'NONE', *, *, #13911, .F. ) ;
#18780 = ( CONVERSION_BASED_UNIT ( 'INCH', #3095 ) LENGTH_UNIT ( ) NAMED_UNIT ( #2933 ) ) ;
#18781 = DIRECTION ( 'NONE',  ( -1.000000000000000000, 0.000000000000000000, 0.000000000000000000 ) ) ;
#18782 = ORIENTED_EDGE ( 'NONE', *, *, #22804, .F. ) ;
#18783 = CIRCLE ( 'NONE', #11133, 0.4921259842519685179 ) ;
#18784 = DIRECTION ( 'NONE',  ( 0.000000000000000000, 0.000000000000000000, 1.000000000000000000 ) ) ;
#18785 = CARTESIAN_POINT ( 'NONE',  ( -0.5511811023622047445, 0.03607471876259063515, 0.9202755905511811330 ) ) ;
#18786 = DIRECTION ( 'NONE',  ( 1.000000000000000000, 0.000000000000000000, 0.000000000000000000 ) ) ;
#18787 = ORIENTED_EDGE ( 'NONE', *, *, #19106, .T. ) ;
#18788 = ( NAMED_UNIT ( * ) SI_UNIT ( $, .STERADIAN. ) SOLID_ANGLE_UNIT ( ) ) ;
#18789 = CARTESIAN_POINT ( 'NONE',  ( 0.000000000000000000, 0.000000000000000000, 2.426181102355854158 ) ) ;
#18790 = EDGE_CURVE ( 'NONE', #8220, #6378, #340, .T. ) ;
#18791 = CARTESIAN_POINT ( 'NONE',  ( -0.09842519685039385902, 0.2165354330708661457, -3.561114497143080815 ) ) ;
#18792 = ORIENTED_EDGE ( 'NONE', *, *, #22959, .F. ) ;
#18793 = CARTESIAN_POINT ( 'NONE',  ( -0.6342142812989975953, 0.1111449751019639998, 0.2359405056180666482 ) ) ;
#18794 = CARTESIAN_POINT ( 'NONE',  ( 0.4857079805366297243, -0.1648275707506031140, -1.550196850393700254 ) ) ;
#18795 = ORIENTED_EDGE ( 'NONE', *, *, #7913, .T. ) ;
#18796 = CARTESIAN_POINT ( 'NONE',  ( 0.2041304421298423266, 0.2660793235464414264, 1.953740157480315043 ) ) ;
#18797 = CARTESIAN_POINT ( 'NONE',  ( 0.2268096725200246799, -0.4600326175569940945, -1.550196850393700920 ) ) ;
#18798 = EDGE_CURVE ( 'NONE', #762, #22736, #14559, .T. ) ;
#18799 = FACE_OUTER_BOUND ( 'NONE', #24922, .T. ) ;
#18800 = AXIS2_PLACEMENT_3D ( 'NONE', #14082, #24806, #26788 ) ;
#18801 = CARTESIAN_POINT ( 'NONE',  ( -0.1775991818008371415, -0.5230301363771194811, 0.9399606299212598381 ) ) ;
#18802 = EDGE_CURVE ( 'NONE', #25409, #4552, #7069, .T. ) ;
#18803 = CARTESIAN_POINT ( 'NONE',  ( 0.5869493968219645641, 0.000000000000000000, 0.000000000000000000 ) ) ;
#18804 = ( GEOMETRIC_REPRESENTATION_CONTEXT ( 3 ) GLOBAL_UNCERTAINTY_ASSIGNED_CONTEXT ( ( #20341 ) ) GLOBAL_UNIT_ASSIGNED_CONTEXT ( ( #21616, #8205, #25711 ) ) REPRESENTATION_CONTEXT ( 'NONE', 'WORKASPACE' ) ) ;
#18805 = ORIENTED_EDGE ( 'NONE', *, *, #26360, .T. ) ;
#18806 = PRODUCT_DEFINITION_SHAPE ( 'NONE', 'NONE',  #19482 ) ;
#18807 = DIRECTION ( 'NONE',  ( 1.000000000000000000, 0.000000000000000000, 0.000000000000000000 ) ) ;
#18808 = ADVANCED_FACE ( 'NONE', ( #6434 ), #1904, .F. ) ;
#18809 = ADVANCED_FACE ( 'NONE', ( #20107 ), #26596, .T. ) ;
#18810 = ORIENTED_EDGE ( 'NONE', *, *, #26814, .F. ) ;
#18811 = CARTESIAN_POINT ( 'NONE',  ( -0.4270824798167792147, -0.2466292688015026546, -1.550196850393700920 ) ) ;
#18812 = VERTEX_POINT ( 'NONE', #3414 ) ;
#18813 = DIRECTION ( 'NONE',  ( -0.7071067811865470176, -0.7071067811865480168, 0.000000000000000000 ) ) ;
#18814 = LINE ( 'NONE', #5846, #12009 ) ;
#18815 = DIRECTION ( 'NONE',  ( 1.000000000000000000, 0.000000000000000000, 0.000000000000000000 ) ) ;
#18816 = CARTESIAN_POINT ( 'NONE',  ( -0.06947563356185801342, -0.5280876769849813801, 1.747047244094488194 ) ) ;
#18817 = ORIENTED_EDGE ( 'NONE', *, *, #12680, .T. ) ;
#18818 = CARTESIAN_POINT ( 'NONE',  ( -0.5626607827700350617, -0.5839868939222687683, 0.9562171551394879065 ) ) ;
#18819 = EDGE_LOOP ( 'NONE', ( #9999, #24043 ) ) ;
#18820 = CARTESIAN_POINT ( 'NONE',  ( -0.6016343471712377600, -0.5391005349154589510, -0.9826765462749172952 ) ) ;
#18821 = DIRECTION ( 'NONE',  ( 0.000000000000000000, 0.000000000000000000, 1.000000000000000000 ) ) ;
#18822 = CARTESIAN_POINT ( 'NONE',  ( 0.000000000000000000, 0.000000000000000000, 0.3543307086614173040 ) ) ;
#18823 = CARTESIAN_POINT ( 'NONE',  ( 0.1198326771653543399, 0.000000000000000000, 0.000000000000000000 ) ) ;
#18824 = ORIENTED_EDGE ( 'NONE', *, *, #15925, .F. ) ;
#18825 = AXIS2_PLACEMENT_3D ( 'NONE', #24337, #757, #11907 ) ;
#18826 = CARTESIAN_POINT ( 'NONE',  ( -0.3149606299212598381, 0.000000000000000000, 0.4330708661417322913 ) ) ;
#18827 = ORIENTED_EDGE ( 'NONE', *, *, #3452, .T. ) ;
#18828 = CARTESIAN_POINT ( 'NONE',  ( 0.3574989824755537837, -0.02345921195965521011, -3.115157480314960647 ) ) ;
#18829 = DIRECTION ( 'NONE',  ( 0.000000000000000000, 0.000000000000000000, -1.000000000000000000 ) ) ;
#18830 = ORIENTED_EDGE ( 'NONE', *, *, #8358, .T. ) ;
#18831 = CARTESIAN_POINT ( 'NONE',  ( -0.1173917140416340377, 0.4382752542996236622, -1.934055118110236338 ) ) ;
#18832 = EDGE_CURVE ( 'NONE', #5287, #17093, #21938, .T. ) ;
#18833 = EDGE_CURVE ( 'NONE', #10143, #6364, #1225, .T. ) ;
#18834 = AXIS2_PLACEMENT_3D ( 'NONE', #1129, #11850, #16102 ) ;
#18835 = VERTEX_POINT ( 'NONE', #17959 ) ;
#18836 = VERTEX_POINT ( 'NONE', #910 ) ;
#18837 = AXIS2_PLACEMENT_3D ( 'NONE', #11536, #20152, #14200 ) ;
#18838 = CARTESIAN_POINT ( 'NONE',  ( -0.4609540795476803621, -0.7091159375545984522, 0.02443766350357295600 ) ) ;
#18839 = ( NAMED_UNIT ( * ) SI_UNIT ( $, .STERADIAN. ) SOLID_ANGLE_UNIT ( ) ) ;
#18840 = CARTESIAN_POINT ( 'NONE',  ( -0.4225965726692971769, 0.3242071728275127129, 1.747047244094488194 ) ) ;
#18841 = CYLINDRICAL_SURFACE ( 'NONE', #24219, 0.6212598425196850238 ) ;
#18842 = ORIENTED_EDGE ( 'NONE', *, *, #5, .T. ) ;
#18843 = ORIENTED_EDGE ( 'NONE', *, *, #10208, .T. ) ;
#18844 = CARTESIAN_POINT ( 'NONE',  ( 0.07874015748031495954, 0.04546065111729338803, -0.3779527559055118058 ) ) ;
#18845 = DIRECTION ( 'NONE',  ( 0.000000000000000000, 0.000000000000000000, 1.000000000000000000 ) ) ;
#18846 = CARTESIAN_POINT ( 'NONE',  ( 0.2208527687086046520, -0.6048181665998788592, 0.2359405056165906622 ) ) ;
#18847 = CARTESIAN_POINT ( 'NONE',  ( 0.3184841198566381593, 0.1570220809524529026, 1.953740157480315043 ) ) ;
#18848 = EDGE_CURVE ( 'NONE', #17724, #25308, #4812, .T. ) ;
#18849 = ORIENTED_EDGE ( 'NONE', *, *, #18731, .F. ) ;
#18850 = EDGE_LOOP ( 'NONE', ( #15353, #9945, #13549, #5144 ) ) ;
#18851 = CARTESIAN_POINT ( 'NONE',  ( -0.4869030747914831481, -0.3865778435145336145, -0.3331566184376838491 ) ) ;
#18852 = CARTESIAN_POINT ( 'NONE',  ( -0.4783464566929133688, 0.9448818897637796255, -0.1771653543307086520 ) ) ;
#18854 = CARTESIAN_POINT ( 'NONE',  ( 0.07214854559198032036, -0.5476281405333571772, 0.9399606299212598381 ) ) ;
#18853 = CARTESIAN_POINT ( 'NONE',  ( 0.5007874015748031704, 0.000000000000000000, 0.2574803149606298969 ) ) ;
#18855 = FACE_BOUND ( 'NONE', #7788, .T. ) ;
#18856 = ORIENTED_EDGE ( 'NONE', *, *, #19680, .F. ) ;
#18857 = VERTEX_POINT ( 'NONE', #26736 ) ;
#18858 = PLANE ( 'NONE',  #13126 ) ;
#18859 = FACE_OUTER_BOUND ( 'NONE', #2758, .T. ) ;
#18860 = AXIS2_PLACEMENT_3D ( 'NONE', #15526, #11535, #812 ) ;
#18861 = B_SPLINE_CURVE_WITH_KNOTS ( 'NONE', 2,
 ( #8027, #18586, #21150 ),
 .UNSPECIFIED., .F., .F.,
 ( 3, 3 ),
 ( 0.000000000000000000, 1.000000000000000000 ),
 .UNSPECIFIED. ) ;
#18862 = VECTOR ( 'NONE', #11475, 39.37007874015748143 ) ;
#18863 = CARTESIAN_POINT ( 'NONE',  ( 0.04679574315772527804, -0.3551931031211721379, -3.115157480314960647 ) ) ;
#18864 = DIRECTION ( 'NONE',  ( 0.000000000000000000, 0.000000000000000000, -1.000000000000000000 ) ) ;
#18865 = AXIS2_PLACEMENT_3D ( 'NONE', #6969, #15181, #21667 ) ;
#18866 = DIRECTION ( 'NONE',  ( -0.000000000000000000, -1.000000000000000000, -0.000000000000000000 ) ) ;
#18867 = DIRECTION ( 'NONE',  ( 0.000000000000000000, -1.000000000000000000, 0.000000000000000000 ) ) ;
#18868 = CARTESIAN_POINT ( 'NONE',  ( -0.09842519685039370636, 2.800920866141732248E-17, 0.09092130223458683158 ) ) ;
#18869 = EDGE_CURVE ( 'NONE', #1935, #10221, #26023, .T. ) ;
#18870 = CARTESIAN_POINT ( 'NONE',  ( 0.0006832381873102289253, 0.6614169699453786855, 0.1616495878897075689 ) ) ;
#18871 = EDGE_CURVE ( 'NONE', #3411, #25722, #1361, .T. ) ;
#18872 = ORIENTED_EDGE ( 'NONE', *, *, #5090, .F. ) ;
#18873 = CARTESIAN_POINT ( 'NONE',  ( -0.0005939837304750000086, 0.5007870493127504208, 0.09685039370078740717 ) ) ;
#18874 = FACE_OUTER_BOUND ( 'NONE', #11770, .T. ) ;
#18875 = CARTESIAN_POINT ( 'NONE',  ( 0.3412792617076850221, 0.05967164814832588010, 0.1377952755905512139 ) ) ;
#18876 = LENGTH_MEASURE_WITH_UNIT ( LENGTH_MEASURE( 0.02539999999999999897 ), #1797 ) ;
#18877 = DIRECTION ( 'NONE',  ( -1.000000000000000000, 0.000000000000000000, 0.000000000000000000 ) ) ;
#18878 = CARTESIAN_POINT ( 'NONE',  ( 0.000000000000000000, 0.4143733464566928815, 0.000000000000000000 ) ) ;
#18879 = CARTESIAN_POINT ( 'NONE',  ( 0.5118110236220472231, 0.03349795313260757468, 1.747047244094488194 ) ) ;
#18880 = VECTOR ( 'NONE', #1236, 39.37007874015748143 ) ;
#18881 = ORIENTED_EDGE ( 'NONE', *, *, #2646, .T. ) ;
#18882 = VERTEX_POINT ( 'NONE', #16299 ) ;
#18883 = CIRCLE ( 'NONE', #27026, 0.4941010236220472751 ) ;
#18884 = DIRECTION ( 'NONE',  ( 0.000000000000000000, 0.000000000000000000, 1.000000000000000000 ) ) ;
#18885 = EDGE_LOOP ( 'NONE', ( #22721, #19369, #5475, #12880 ) ) ;
#18886 = VECTOR ( 'NONE', #26837, 39.37007874015748143 ) ;
#18887 = CARTESIAN_POINT ( 'NONE',  ( -0.4143937130615245046, 0.4928070724629356469, 0.2359405056176802906 ) ) ;
#18888 = CARTESIAN_POINT ( 'NONE',  ( -0.0004986409324230409688, 0.3484797321218884303, 0.1166443193928871913 ) ) ;
#18889 = CARTESIAN_POINT ( 'NONE',  ( -0.2041304421298332783, 0.2660793235464289364, 1.973425196850393970 ) ) ;
#18890 = EDGE_CURVE ( 'NONE', #8023, #25040, #16106, .T. ) ;
#18891 = VERTEX_POINT ( 'NONE', #26884 ) ;
#18892 = CARTESIAN_POINT ( 'NONE',  ( -0.1275996891957763835, -0.4763861460130486281, -1.550196850393700920 ) ) ;
#18893 = CYLINDRICAL_SURFACE ( 'NONE', #10963, 0.2952755905264887182 ) ;
#18894 = AXIS2_PLACEMENT_3D ( 'NONE', #4454, #24080, #2460 ) ;
#18895 = ORIENTED_EDGE ( 'NONE', *, *, #17550, .T. ) ;
#18896 = ORIENTED_EDGE ( 'NONE', *, *, #5527, .T. ) ;
#18897 = EDGE_LOOP ( 'NONE', ( #23723, #1121 ) ) ;
#18898 = VERTEX_POINT ( 'NONE', #22978 ) ;
#18899 = CARTESIAN_POINT ( 'NONE',  ( -0.3726024258163779246, 0.000000000000000000, -3.115157480314960647 ) ) ;
#18900 = CARTESIAN_POINT ( 'NONE',  ( -0.2420394123212937232, 0.2892587550802429575, 0.1992125984251968684 ) ) ;
#18901 = DIRECTION ( 'NONE',  ( 0.000000000000000000, -1.000000000000000000, 0.000000000000000000 ) ) ;
#18902 = CARTESIAN_POINT ( 'NONE',  ( 0.1707210962531913734, -0.4707890492249701131, 0.2574803149606298969 ) ) ;
#18903 = B_SPLINE_CURVE_WITH_KNOTS ( 'NONE', 3,
 ( #5964, #25155, #12029, #9761, #22911, #12303 ),
 .UNSPECIFIED., .F., .F.,
 ( 4, 2, 4 ),
 ( 0.5000000000000000000, 0.7500000000000000000, 1.000000000000000000 ),
 .UNSPECIFIED. ) ;
#18904 = CIRCLE ( 'NONE', #1314, 0.1181102362204724532 ) ;
#18905 = ORIENTED_EDGE ( 'NONE', *, *, #13446, .T. ) ;
#18906 = CARTESIAN_POINT ( 'NONE',  ( -0.3759206409296168561, 0.2989751379763687655, 0.2362204724409447676 ) ) ;
#18907 = CIRCLE ( 'NONE', #12612, 0.06200787401574745644 ) ;
#18908 = EDGE_CURVE ( 'NONE', #19141, #27334, #3923, .T. ) ;
#18909 = DIRECTION ( 'NONE',  ( -1.000000000000000000, 0.000000000000000000, 0.000000000000000000 ) ) ;
#18910 = CYLINDRICAL_SURFACE ( 'NONE', #27706, 0.1771653543307086520 ) ;
#18911 = CARTESIAN_POINT ( 'NONE',  ( -1.355511558298621910, 1.564461769117756029, 2.145669291338582862 ) ) ;
#18912 = EDGE_CURVE ( 'NONE', #24718, #9254, #19877, .T. ) ;
#18913 = CARTESIAN_POINT ( 'NONE',  ( -0.5536325768349827925, -0.3642082843426176497, 0.1838265301724124334 ) ) ;
#18914 = CARTESIAN_POINT ( 'NONE',  ( -0.1771653543307086520, -0.6299212598425196763, 7.714310545810098438E-17 ) ) ;
#18915 = DIRECTION ( 'NONE',  ( 0.000000000000000000, 0.000000000000000000, -1.000000000000000000 ) ) ;
#18916 = PRESENTATION_LAYER_ASSIGNMENT (  '', '', ( #4915 ) ) ;
#18917 = DIRECTION ( 'NONE',  ( 0.000000000000000000, 0.000000000000000000, 1.000000000000000000 ) ) ;
#18918 = DIRECTION ( 'NONE',  ( 0.7071067818211390632, 0.000000000000000000, 0.7071067805519560823 ) ) ;
#18919 = DIMENSIONAL_EXPONENTS ( 1.000000000000000000, 0.000000000000000000, 0.000000000000000000, 0.000000000000000000, 0.000000000000000000, 0.000000000000000000, 0.000000000000000000 ) ;
#18920 = DIRECTION ( 'NONE',  ( 0.7071067818211385081, -0.7071067805519564153, 0.000000000000000000 ) ) ;
#18921 = B_SPLINE_CURVE_WITH_KNOTS ( 'NONE', 3,
 ( #64, #17384, #8897, #12861, #15284, #26139 ),
 .UNSPECIFIED., .F., .F.,
 ( 4, 2, 4 ),
 ( 0.3864984308775630262, 0.3881911340211369743, 0.3898838371647120327 ),
 .UNSPECIFIED. ) ;
#18922 = CARTESIAN_POINT ( 'NONE',  ( 0.3593781546376668135, 4.401113067605012182E-17, -0.2755905511811023723 ) ) ;
#18923 = ORIENTED_EDGE ( 'NONE', *, *, #20993, .T. ) ;
#18924 = EDGE_LOOP ( 'NONE', ( #18399, #1200, #18805, #21987 ) ) ;
#18925 = CARTESIAN_POINT ( 'NONE',  ( -0.03937007874015747977, -0.8267716535433071723, 1.012503259137575512E-16 ) ) ;
#18926 = ( NAMED_UNIT ( * ) PLANE_ANGLE_UNIT ( ) SI_UNIT ( $, .RADIAN. ) ) ;
#18927 = CARTESIAN_POINT ( 'NONE',  ( 0.000000000000000000, 0.000000000000000000, -0.1111195235210984261 ) ) ;
#18928 = ORIENTED_EDGE ( 'NONE', *, *, #14932, .T. ) ;
#18929 = VERTEX_POINT ( 'NONE', #16344 ) ;
#18930 = CARTESIAN_POINT ( 'NONE',  ( 0.000000000000000000, 0.9055118110236221041, -0.4921259842519685179 ) ) ;
#18931 = CARTESIAN_POINT ( 'NONE',  ( 0.000000000000000000, 0.000000000000000000, -0.1309055118110236116 ) ) ;
#18933 = CARTESIAN_POINT ( 'NONE',  ( -0.4783323773986817851, 0.2762247810518556612, 0.9202755905511811330 ) ) ;
#18932 = AXIS2_PLACEMENT_3D ( 'NONE', #2523, #13396, #19483 ) ;
#18934 = EDGE_LOOP ( 'NONE', ( #26567, #26219 ) ) ;
#18935 = DIRECTION ( 'NONE',  ( 0.000000000000000000, 0.000000000000000000, -1.000000000000000000 ) ) ;
#18936 = ORIENTED_EDGE ( 'NONE', *, *, #27793, .T. ) ;
#18937 = ADVANCED_FACE ( 'NONE', ( #9834, #18573 ), #809, .T. ) ;
#18938 = CARTESIAN_POINT ( 'NONE',  ( 9.591958661417321355E-18, 0.000000000000000000, -3.978489941880726022 ) ) ;
#18939 = LINE ( 'NONE', #22913, #4643 ) ;
#18940 = ORIENTED_EDGE ( 'NONE', *, *, #17078, .F. ) ;
#18941 = CARTESIAN_POINT ( 'NONE',  ( -7.279147705782180972E-18, 0.5322834645669292097, 0.1322810039474933141 ) ) ;
#18942 = DIRECTION ( 'NONE',  ( 0.000000000000000000, 1.000000000000000000, 0.000000000000000000 ) ) ;
#18943 = ADVANCED_FACE ( 'NONE', ( #4399 ), #2110, .F. ) ;
#18944 = ORIENTED_EDGE ( 'NONE', *, *, #21767, .F. ) ;
#18945 = CARTESIAN_POINT ( 'NONE',  ( 0.1677079028045344034, -0.2904160862623691997, 1.973425196850393970 ) ) ;
#18946 = DIRECTION ( 'NONE',  ( -1.000000000000000000, 0.000000000000000000, 0.000000000000000000 ) ) ;
#18947 = AXIS2_PLACEMENT_3D ( 'NONE', #15810, #26821, #15679 ) ;
#18948 = SPHERICAL_SURFACE ( 'NONE', #23282, 0.07677362204724409722 ) ;
#18949 = DIRECTION ( 'NONE',  ( -0.2036417511401760472, 0.4895227362422920336, 0.8478782506317883438 ) ) ;
#18950 = AXIS2_PLACEMENT_3D ( 'NONE', #16659, #6216, #14844 ) ;
#18951 = CARTESIAN_POINT ( 'NONE',  ( -0.5511811023622048555, 0.000000000000000000, 0.9399606299212598381 ) ) ;
#18952 = DIRECTION ( 'NONE',  ( -1.000000000000000000, 0.000000000000000000, 0.000000000000000000 ) ) ;
#18953 = ORIENTED_EDGE ( 'NONE', *, *, #1906, .T. ) ;
#18954 = CARTESIAN_POINT ( 'NONE',  ( -0.1968503937007874127, 0.07874015748031495954, 0.04546065111729331171 ) ) ;
#18955 = AXIS2_PLACEMENT_3D ( 'NONE', #12585, #25441, #3376 ) ;
#18956 = ORIENTED_EDGE ( 'NONE', *, *, #25516, .F. ) ;
#18957 = B_SPLINE_CURVE_WITH_KNOTS ( 'NONE', 3,
 ( #3511, #25282, #18306, #5481, #9848, #27375 ),
 .UNSPECIFIED., .F., .F.,
 ( 4, 2, 4 ),
 ( 0.5000000000000000000, 0.7500000000000000000, 1.000000000000000000 ),
 .UNSPECIFIED. ) ;
#18958 = CARTESIAN_POINT ( 'NONE',  ( -0.5118110236220473341, 0.000000000000000000, -1.550196850393700920 ) ) ;
#18959 = CARTESIAN_POINT ( 'NONE',  ( -0.7086614173228346081, 0.000000000000000000, 1.555118110236220597 ) ) ;
#18960 = CARTESIAN_POINT ( 'NONE',  ( 0.03532354024591842501, -0.6299212598425195653, 0.6299212598425196763 ) ) ;
#18961 = DIRECTION ( 'NONE',  ( 0.000000000000000000, 1.000000000000000000, 0.000000000000000000 ) ) ;
#18962 = ADVANCED_FACE ( 'NONE', ( #8496 ), #24203, .F. ) ;
#18963 = EDGE_CURVE ( 'NONE', #2754, #13649, #14786, .T. ) ;
#18964 = ORIENTED_EDGE ( 'NONE', *, *, #12829, .T. ) ;
#18965 = CARTESIAN_POINT ( 'NONE',  ( -0.5905511811023621549, -0.6348133144914153148, 0.8891632684400255782 ) ) ;
#18966 = EDGE_LOOP ( 'NONE', ( #1155, #4103, #10199, #9146 ) ) ;
#18967 = EDGE_CURVE ( 'NONE', #14646, #13130, #10671, .T. ) ;
#18968 = CARTESIAN_POINT ( 'NONE',  ( 0.2299571666351564181, 0.2748389102007000040, 0.09506557084325908957 ) ) ;
#18969 = TOROIDAL_SURFACE ( 'NONE', #18503, 0.1476377952755905387, 0.01968503937007873988 ) ;
#18970 = FACE_OUTER_BOUND ( 'NONE', #4918, .T. ) ;
#18971 = CARTESIAN_POINT ( 'NONE',  ( 0.000000000000000000, 0.9055118110236221041, 0.000000000000000000 ) ) ;
#18972 = CYLINDRICAL_SURFACE ( 'NONE', #1871, 0.5007874015748031704 ) ;
#18973 = EDGE_CURVE ( 'NONE', #26390, #8702, #2552, .T. ) ;
#18974 = ORIENTED_EDGE ( 'NONE', *, *, #838, .F. ) ;
#18975 = DIRECTION ( 'NONE',  ( 0.000000000000000000, 1.000000000000000000, 0.000000000000000000 ) ) ;
#18976 = TOROIDAL_SURFACE ( 'NONE', #6352, 0.5610236220472440971, 0.1003937007874015908 ) ;
#18977 = DIRECTION ( 'NONE',  ( 1.000000000000000000, 0.000000000000000000, 0.000000000000000000 ) ) ;
#18978 = ADVANCED_FACE ( 'NONE', ( #18439 ), #19245, .F. ) ;
#18979 = ORIENTED_EDGE ( 'NONE', *, *, #10619, .T. ) ;
#18980 = CARTESIAN_POINT ( 'NONE',  ( 0.3574975638436101444, 4.268512490100411279E-17, -3.115157480314960647 ) ) ;
#18981 = PLANE ( 'NONE',  #2632 ) ;
#18982 = DIMENSIONAL_EXPONENTS ( 1.000000000000000000, 0.000000000000000000, 0.000000000000000000, 0.000000000000000000, 0.000000000000000000, 0.000000000000000000, 0.000000000000000000 ) ;
#18983 = CARTESIAN_POINT ( 'NONE',  ( -0.4498374011143459472, -0.05926487674658267174, -1.934055118110236338 ) ) ;
#18984 = CARTESIAN_POINT ( 'NONE',  ( 0.3012109481301854519, 0.3598698725862389813, 0.1992125984251968684 ) ) ;
#18985 = AXIS2_PLACEMENT_3D ( 'NONE', #15359, #1918, #17449 ) ;
#18986 = VERTEX_POINT ( 'NONE', #3471 ) ;
#18987 = EDGE_LOOP ( 'NONE', ( #23334, #20984, #3795, #16599 ) ) ;
#18988 = ORIENTED_EDGE ( 'NONE', *, *, #7076, .F. ) ;
#18989 = CARTESIAN_POINT ( 'NONE',  ( -0.5935113537020059171, -0.1956639913954956733, 0.06179785775180177826 ) ) ;
#18990 = LENGTH_MEASURE_WITH_UNIT ( LENGTH_MEASURE( 0.02539999999999999897 ), #6290 ) ;
#18991 = CARTESIAN_POINT ( 'NONE',  ( 0.06699507805368110080, -0.5085118447801203478, 1.747047244094488194 ) ) ;
#18992 = ORIENTED_EDGE ( 'NONE', *, *, #10679, .T. ) ;
#18993 = CARTESIAN_POINT ( 'NONE',  ( 0.7871730179869350641, 0.2557924603611196890, -0.2773276354978094771 ) ) ;
#18994 = VERTEX_POINT ( 'NONE', #18580 ) ;
#18995 = DIRECTION ( 'NONE',  ( 1.000000000000000000, 0.000000000000000000, 0.000000000000000000 ) ) ;
#18996 = B_SPLINE_CURVE_WITH_KNOTS ( 'NONE', 3,
 ( #23577, #1525, #5918, #3783, #12404, #21018, #10272, #18887, #16784, #25397 ),
 .UNSPECIFIED., .F., .F.,
 ( 4, 2, 2, 2, 4 ),
 ( 0.000000000000000000, 0.2500000000000000000, 0.5000000000000000000, 0.7500000000000000000, 1.000000000000000000 ),
 .UNSPECIFIED. ) ;
#18997 = DIRECTION ( 'NONE',  ( 0.000000000000000000, -1.000000000000000000, 0.000000000000000000 ) ) ;
#18998 = CARTESIAN_POINT ( 'NONE',  ( 0.4303653410901771004, 0.1153552079391450824, -1.934055118110237004 ) ) ;
#18999 = EDGE_LOOP ( 'NONE', ( #18944, #17212, #22404, #19899 ) ) ;
#19000 = CARTESIAN_POINT ( 'NONE',  ( -0.3520466617656974884, -0.04638120790932648285, 1.953740157480315043 ) ) ;
#19001 = EDGE_LOOP ( 'NONE', ( #18630, #11344, #21839, #12054 ) ) ;
#19002 = CARTESIAN_POINT ( 'NONE',  ( -0.5390321293728450591, -0.2641768698347569111, -0.2800551229596216496 ) ) ;
#19003 = CARTESIAN_POINT ( 'NONE',  ( 0.4061284506583976994, -0.2351468520617074898, 0.1992125984251968684 ) ) ;
#19004 = ( REPRESENTATION_RELATIONSHIP ('NONE','NONE', #12434, #6338 ) REPRESENTATION_RELATIONSHIP_WITH_TRANSFORMATION ( #9434 )SHAPE_REPRESENTATION_RELATIONSHIP( ) ) ;
#19005 = ORIENTED_EDGE ( 'NONE', *, *, #8506, .T. ) ;
#19006 = APPLICATION_CONTEXT ( 'automotive_design' ) ;
#19007 = DIRECTION ( 'NONE',  ( 0.2036417511401769909, 0.4895227362422910344, -0.8478782506317890100 ) ) ;
#19008 = CARTESIAN_POINT ( 'NONE',  ( -0.2362204724409449064, 0.000000000000000000, 0.000000000000000000 ) ) ;
#19009 = EDGE_CURVE ( 'NONE', #9793, #5280, #6636, .T. ) ;
#19010 = AXIS2_PLACEMENT_3D ( 'NONE', #19915, #23383, #567 ) ;
#19011 = CARTESIAN_POINT ( 'NONE',  ( 0.2842490391651533721, -0.2180698645301867300, -3.115157480314960647 ) ) ;
#19012 = EDGE_CURVE ( 'NONE', #16931, #339, #19529, .T. ) ;
#19013 = LINE ( 'NONE', #5898, #18880 ) ;
#19014 = CARTESIAN_POINT ( 'NONE',  ( 0.5314960629921260393, 0.000000000000000000, 1.747047244094488194 ) ) ;
#19015 = AXIS2_PLACEMENT_3D ( 'NONE', #24101, #11237, #8976 ) ;
#19016 = CARTESIAN_POINT ( 'NONE',  ( 0.0005896702191549359900, 0.4865884552403887398, 0.1827409795202793175 ) ) ;
#19017 = AXIS2_PLACEMENT_3D ( 'NONE', #17025, #1345, #12076 ) ;
#19018 = DIRECTION ( 'NONE',  ( 0.000000000000000000, 1.000000000000000000, 0.000000000000000000 ) ) ;
#19019 = EDGE_CURVE ( 'NONE', #27336, #7980, #6086, .T. ) ;
#19020 = EDGE_LOOP ( 'NONE', ( #18123, #8551, #10094, #15809 ) ) ;
#19021 = CARTESIAN_POINT ( 'NONE',  ( 0.1838445375787389757, 0.5417516942597615515, 0.9399606299212601712 ) ) ;
#19022 = VERTEX_POINT ( 'NONE', #4538 ) ;
#19023 = CARTESIAN_POINT ( 'NONE',  ( -0.6995386212070490162, 0.5414171171806005933, -0.4387325693061223664 ) ) ;
#19024 = CARTESIAN_POINT ( 'NONE',  ( 0.01288382813972203597, 0.2165354330708660902, -3.646653543307087020 ) ) ;
#19025 = CARTESIAN_POINT ( 'NONE',  ( -0.3020979083623086536, 0.3591256245825952265, 0.07637795275590551769 ) ) ;
#19026 = PLANE ( 'NONE',  #8890 ) ;
#19027 = ORIENTED_EDGE ( 'NONE', *, *, #15401, .F. ) ;
#19028 = AXIS2_PLACEMENT_3D ( 'NONE', #5822, #14747, #23353 ) ;
#19029 = VERTEX_POINT ( 'NONE', #9039 ) ;
#19030 = CARTESIAN_POINT ( 'NONE',  ( -0.2362439534887390002, -0.2693339498142257038, -3.115157480314960647 ) ) ;
#19031 = FACE_BOUND ( 'NONE', #25995, .T. ) ;
#19032 = ( LENGTH_UNIT ( ) NAMED_UNIT ( * ) SI_UNIT ( $, .METRE. ) ) ;
#19033 = CARTESIAN_POINT ( 'NONE',  ( 0.3976891862754212137, 1.133679329692560911, -0.4395307839725692833 ) ) ;
#19034 = CARTESIAN_POINT ( 'NONE',  ( 0.1482986320106470801, -0.3007905576423859917, 1.973425196850393970 ) ) ;
#19035 = VERTEX_POINT ( 'NONE', #10803 ) ;
#19036 = VERTEX_POINT ( 'NONE', #26810 ) ;
#19037 = EDGE_CURVE ( 'NONE', #22996, #12810, #17451, .T. ) ;
#19038 = CIRCLE ( 'NONE', #5035, 0.1082677165354330312 ) ;
#19039 = CARTESIAN_POINT ( 'NONE',  ( -0.1275996891957738577, 0.4763861460130593972, -1.550196850393700920 ) ) ;
#19040 = ORIENTED_EDGE ( 'NONE', *, *, #24013, .F. ) ;
#19041 = ORIENTED_EDGE ( 'NONE', *, *, #7983, .T. ) ;
#19042 = EDGE_CURVE ( 'NONE', #1699, #9929, #9779, .T. ) ;
#19043 = DIRECTION ( 'NONE',  ( 0.000000000000000000, 0.000000000000000000, 1.000000000000000000 ) ) ;
#19044 = CARTESIAN_POINT ( 'NONE',  ( 0.2128972891168661452, -0.5836425148029424914, 0.09684874924366436433 ) ) ;
#19045 = DIRECTION ( 'NONE',  ( -0.000000000000000000, -1.000000000000000000, -0.000000000000000000 ) ) ;
#19046 = B_SPLINE_SURFACE_WITH_KNOTS ( 'NONE', 3, 3, ( 
 ( #14832, #14964, #6469, #19033 ),
 ( #23713, #6063, #25684, #12817 ),
 ( #21449, #20, #4074, #8585 ),
 ( #17202, #2221, #10842, #19456 ) ),
 .UNSPECIFIED., .F., .F., .F.,
 ( 4, 4 ),
 ( 4, 4 ),
 ( 0.000000000000000000, 1.000000000000000000 ),
 ( -1.199999999999999956, 0.000000000000000000 ),
 .UNSPECIFIED. ) ;
#19047 = AXIS2_PLACEMENT_3D ( 'NONE', #4489, #149, #2350 ) ;
#19048 = ORIENTED_EDGE ( 'NONE', *, *, #17017, .T. ) ;
#19049 = DIRECTION ( 'NONE',  ( -1.000000000000000000, 0.000000000000000000, 0.000000000000000000 ) ) ;
#19050 = AXIS2_PLACEMENT_3D ( 'NONE', #2380, #24271, #15801 ) ;
#19051 = DIRECTION ( 'NONE',  ( 1.000000000000000000, 0.000000000000000000, 0.000000000000000000 ) ) ;
#19052 = LINE ( 'NONE', #16670, #13705 ) ;
#19053 = ( LENGTH_UNIT ( ) NAMED_UNIT ( * ) SI_UNIT ( $, .METRE. ) ) ;
#19054 = AXIS2_PLACEMENT_3D ( 'NONE', #4864, #19721, #9230 ) ;
#19055 = CARTESIAN_POINT ( 'NONE',  ( -0.6027608817597299717, -0.1906417529132624356, 0.2220433626720438591 ) ) ;
#19056 = CARTESIAN_POINT ( 'NONE',  ( 0.000000000000000000, 0.000000000000000000, -0.4724409448841456749 ) ) ;
#19057 = CARTESIAN_POINT ( 'NONE',  ( -0.4930758245789425009, 0.08754571829529331217, 0.09685039370078740717 ) ) ;
#19058 = CARTESIAN_POINT ( 'NONE',  ( -0.1968503937007874127, 0.07874015748031495954, 0.04546065111729331171 ) ) ;
#19059 = CARTESIAN_POINT ( 'NONE',  ( 0.1279527559055118058, 0.7713036219899488399, 0.000000000000000000 ) ) ;
#19060 = DIRECTION ( 'NONE',  ( 0.000000000000000000, -1.000000000000000000, 0.000000000000000000 ) ) ;
#19061 = ORIENTED_EDGE ( 'NONE', *, *, #14990, .T. ) ;
#19062 = VERTEX_POINT ( 'NONE', #11420 ) ;
#19063 = DIRECTION ( 'NONE',  ( 0.2036417511401769909, -0.4895227362422910344, 0.8478782506317890100 ) ) ;
#19064 = LENGTH_MEASURE_WITH_UNIT ( LENGTH_MEASURE( 0.02539999999999999897 ), #12985 ) ;
#19065 = DIRECTION ( 'NONE',  ( 0.000000000000000000, -1.000000000000000000, 0.000000000000000000 ) ) ;
#19066 = AXIS2_PLACEMENT_3D ( 'NONE', #27880, #8103, #4004 ) ;
#19067 = EDGE_LOOP ( 'NONE', ( #13722, #15867, #15492, #3780 ) ) ;
#19068 = EDGE_CURVE ( 'NONE', #26373, #12810, #6648, .T. ) ;
#19069 = AXIS2_PLACEMENT_3D ( 'NONE', #10285, #16244, #12130 ) ;
#19070 = CARTESIAN_POINT ( 'NONE',  ( 0.4932821129636645874, 0.08637579872942321990, 0.09685039370078740717 ) ) ;
#19071 = CARTESIAN_POINT ( 'NONE',  ( 0.5525004126151165096, 0.09742072959660433296, 0.1771653543307086520 ) ) ;
#19072 = CARTESIAN_POINT ( 'NONE',  ( 0.4382482975805264136, 0.3362148458988503674, 0.9202755905511811330 ) ) ;
#19073 = EDGE_LOOP ( 'NONE', ( #17232, #1023, #10974, #3860 ) ) ;
#19074 = EDGE_CURVE ( 'NONE', #7850, #4078, #17773, .T. ) ;
#19075 = SPHERICAL_SURFACE ( 'NONE', #7672, 0.07677362204724409722 ) ;
#19076 = ORIENTED_EDGE ( 'NONE', *, *, #25037, .F. ) ;
#19077 = CIRCLE ( 'NONE', #22216, 0.6299212598425196763 ) ;
#19078 = DIRECTION ( 'NONE',  ( 0.000000000000000000, -1.000000000000000000, 0.000000000000000000 ) ) ;
#19079 = CARTESIAN_POINT ( 'NONE',  ( -0.4537304931026617250, 0.07942646906834199827, 0.1903859677797853645 ) ) ;
#19080 = DIRECTION ( 'NONE',  ( 0.000000000000000000, 0.000000000000000000, 1.000000000000000000 ) ) ;
#19081 = ORIENTED_EDGE ( 'NONE', *, *, #1720, .T. ) ;
#19082 = FACE_OUTER_BOUND ( 'NONE', #18706, .T. ) ;
#19083 = ORIENTED_EDGE ( 'NONE', *, *, #3452, .F. ) ;
#19084 = AXIS2_PLACEMENT_3D ( 'NONE', #20073, #9055, #10912 ) ;
#19085 = DIRECTION ( 'NONE',  ( 0.000000000000000000, 0.000000000000000000, 1.000000000000000000 ) ) ;
#19086 = CARTESIAN_POINT ( 'NONE',  ( 0.0005855335178306408407, 0.4865383137630506782, 0.2467937632983550900 ) ) ;
#19087 = TOROIDAL_SURFACE ( 'NONE', #2828, 0.4232283464566928832, 0.07677165354330708902 ) ;
#19088 = CARTESIAN_POINT ( 'NONE',  ( 0.3362148458988509225, -0.4382482975804891101, 0.9399606299212598381 ) ) ;
#19089 = FACE_OUTER_BOUND ( 'NONE', #4, .T. ) ;
#19090 = DIRECTION ( 'NONE',  ( 0.000000000000000000, 1.000000000000000000, 0.000000000000000000 ) ) ;
#19091 = CARTESIAN_POINT ( 'NONE',  ( -1.456051859514965975E-17, 0.4692913385826771866, 0.1992150590373740204 ) ) ;
#19092 = EDGE_LOOP ( 'NONE', ( #26455, #19175, #2345, #4220, #23707, #20385, #5217, #14693, #2343 ) ) ;
#19093 = CARTESIAN_POINT ( 'NONE',  ( 0.3102827802122046230, 0.1791101711255022044, -3.115157480314962424 ) ) ;
#19094 = CIRCLE ( 'NONE', #22704, 0.4842519685039370358 ) ;
#19095 = AXIS2_PLACEMENT_3D ( 'NONE', #20195, #13991, #2948 ) ;
#19096 = LENGTH_MEASURE_WITH_UNIT ( LENGTH_MEASURE( 0.02539999999999999897 ), #14614 ) ;
#19097 = ORIENTED_EDGE ( 'NONE', *, *, #6553, .T. ) ;
#19098 = TOROIDAL_SURFACE ( 'NONE', #26312, 0.7480314960629921295, 0.03937007874015747977 ) ;
#19099 = VERTEX_POINT ( 'NONE', #2251 ) ;
#19100 = CARTESIAN_POINT ( 'NONE',  ( 0.2268096725200246799, -0.4600326175569940945, -1.550196850393700920 ) ) ;
#19101 = ORIENTED_EDGE ( 'NONE', *, *, #7757, .F. ) ;
#19102 = CARTESIAN_POINT ( 'NONE',  ( 0.1481199686343411814, -0.5525886237723267591, 0.9399606299212601712 ) ) ;
#19103 = DIRECTION ( 'NONE',  ( 1.000000000000000000, 0.000000000000000000, 0.000000000000000000 ) ) ;
#19104 = CARTESIAN_POINT ( 'NONE',  ( 0.000000000000000000, -5.394653543307086438E-17, -0.1627508102905848297 ) ) ;
#19105 = CARTESIAN_POINT ( 'NONE',  ( -0.03488411621167891719, -0.5314974819112028293, 1.747047244094488194 ) ) ;
#19106 = EDGE_CURVE ( 'NONE', #19868, #16425, #12925, .T. ) ;
#19107 = CLOSED_SHELL ( 'NONE', ( #11044, #10180, #26396, #25386, #7661, #203, #18749, #8747, #5433, #1568, #14809, #4837, #21560, #934, #23805, #12474, #9345, #4807, #7085, #23505, #16990 ) ) ;
#19108 = DIRECTION ( 'NONE',  ( 0.000000000000000000, 0.000000000000000000, 1.000000000000000000 ) ) ;
#19109 = ORIENTED_EDGE ( 'NONE', *, *, #23992, .T. ) ;
#19110 = FACE_OUTER_BOUND ( 'NONE', #20138, .T. ) ;
#19111 = CARTESIAN_POINT ( 'NONE',  ( 0.000000000000000000, 0.000000000000000000, 0.1771653543307086520 ) ) ;
#19112 = CARTESIAN_POINT ( 'NONE',  ( -0.2362204724409449064, 0.6299212598425196763, 0.000000000000000000 ) ) ;
#19113 = DIRECTION ( 'NONE',  ( 0.000000000000000000, 1.000000000000000000, 0.000000000000000000 ) ) ;
#19114 = CARTESIAN_POINT ( 'NONE',  ( 0.03937007874015747977, 0.000000000000000000, 0.000000000000000000 ) ) ;
#19115 = AXIS2_PLACEMENT_3D ( 'NONE', #25701, #21187, #14849 ) ;
#19116 = CARTESIAN_POINT ( 'NONE',  ( -0.2362204724409449064, -0.4724409448818898127, -0.8182917201112815953 ) ) ;
#19117 = ORIENTED_EDGE ( 'NONE', *, *, #12287, .F. ) ;
#19118 = AXIS2_PLACEMENT_3D ( 'NONE', #18394, #7539, #24906 ) ;
#19119 = VERTEX_POINT ( 'NONE', #183 ) ;
#19120 = CARTESIAN_POINT ( 'NONE',  ( 0.000000000000000000, 0.000000000000000000, -0.05511811023622047168 ) ) ;
#19121 = CARTESIAN_POINT ( 'NONE',  ( -0.4555658499976060760, 0.06001958459474820984, -1.928289503579160513 ) ) ;
#19122 = CARTESIAN_POINT ( 'NONE',  ( 0.4438564651657541105, -0.1188866373884811950, -1.928289503579147857 ) ) ;
#19123 = ADVANCED_FACE ( 'NONE', ( #13399, #17641 ), #23884, .T. ) ;
#19124 = B_SPLINE_CURVE_WITH_KNOTS ( 'NONE', 3,
 ( #20251, #7538, #11920, #26602, #3144, #9649 ),
 .UNSPECIFIED., .F., .F.,
 ( 4, 2, 4 ),
 ( 0.7157687286427140139, 0.7172350147555660582, 0.7187013008684189908 ),
 .UNSPECIFIED. ) ;
#19125 = CIRCLE ( 'NONE', #17343, 0.1308464566929133932 ) ;
#19126 = EDGE_CURVE ( 'NONE', #7494, #24512, #21513, .T. ) ;
#19127 = ORIENTED_EDGE ( 'NONE', *, *, #251, .F. ) ;
#19128 = CARTESIAN_POINT ( 'NONE',  ( -0.5355664161054535244, -0.3246709447438385632, -0.1343123395640568873 ) ) ;
#19129 = B_SPLINE_CURVE_WITH_KNOTS ( 'NONE', 3,
 ( #11375, #9816, #19995, #7143 ),
 .UNSPECIFIED., .F., .F.,
 ( 4, 4 ),
 ( 0.000000000000000000, 0.08984410251848014284 ),
 .UNSPECIFIED. ) ;
#19130 = CARTESIAN_POINT ( 'NONE',  ( 0.3995066426835732765, 0.4757712504659606378, 0.09684793308443542803 ) ) ;
#19131 = ORIENTED_EDGE ( 'NONE', *, *, #15433, .F. ) ;
#19132 = CIRCLE ( 'NONE', #3324, 0.2847264097284254447 ) ;
#19133 = FACE_OUTER_BOUND ( 'NONE', #22066, .T. ) ;
#19134 = CARTESIAN_POINT ( 'NONE',  ( -0.6016344796479202728, -0.5390998427281981087, 0.9826767787459085302 ) ) ;
#19135 = ADVANCED_FACE ( 'NONE', ( #25992 ), #22160, .T. ) ;
#19136 = CIRCLE ( 'NONE', #16894, 0.3722026523000413478 ) ;
#19137 = CARTESIAN_POINT ( 'NONE',  ( -0.5708661417322834497, 0.000000000000000000, 0.9399606299212598381 ) ) ;
#19138 = CARTESIAN_POINT ( 'NONE',  ( -0.01202960507629146324, -0.5140881368932568307, 0.1365555443425394977 ) ) ;
#19139 = ORIENTED_EDGE ( 'NONE', *, *, #20896, .T. ) ;
#19140 = CARTESIAN_POINT ( 'NONE',  ( 0.1141709026133613525, -0.3362336590883617249, 1.953740157480315043 ) ) ;
#19141 = VERTEX_POINT ( 'NONE', #7054 ) ;
#19142 = CARTESIAN_POINT ( 'NONE',  ( -0.5981339658092079681, -0.1309848305394583079, -0.2467760297474455855 ) ) ;
#19143 = DIRECTION ( 'NONE',  ( 0.000000000000000000, 0.000000000000000000, -1.000000000000000000 ) ) ;
#19144 = ORIENTED_EDGE ( 'NONE', *, *, #3504, .F. ) ;
#19145 = ORIENTED_EDGE ( 'NONE', *, *, #18551, .F. ) ;
#19146 = DIRECTION ( 'NONE',  ( 0.000000000000000000, 0.000000000000000000, 1.000000000000000000 ) ) ;
#19147 = CARTESIAN_POINT ( 'NONE',  ( 0.000000000000000000, 0.000000000000000000, 0.4724409448818898127 ) ) ;
#19148 = AXIS2_PLACEMENT_3D ( 'NONE', #1002, #9590, #26413 ) ;
#19149 = CARTESIAN_POINT ( 'NONE',  ( -0.1200583359873150374, -0.3535721684717939017, -3.115157480314960647 ) ) ;
#19150 = DIRECTION ( 'NONE',  ( 1.000000000000000000, 0.000000000000000000, 0.000000000000000000 ) ) ;
#19151 = CARTESIAN_POINT ( 'NONE',  ( 0.4333973147258542991, -0.2509079296564015737, 0.2574803149606298969 ) ) ;
#19152 = CARTESIAN_POINT ( 'NONE',  ( 0.3015429802568458384, -0.1746717017766615809, 0.1589462317943655945 ) ) ;
#19153 = DIRECTION ( 'NONE',  ( 1.000000000000000000, 0.000000000000000000, 0.000000000000000000 ) ) ;
#19154 = DIRECTION ( 'NONE',  ( -0.9396926207859082059, -0.3420201433256691015, 0.000000000000000000 ) ) ;
#19155 = DIRECTION ( 'NONE',  ( 0.000000000000000000, -1.000000000000000000, 0.000000000000000000 ) ) ;
#19156 = VECTOR ( 'NONE', #20856, 39.37007874015748143 ) ;
#19157 = CARTESIAN_POINT ( 'NONE',  ( 0.000000000000000000, 0.3543307086614173040, -0.7874015748031496509 ) ) ;
#19158 = CARTESIAN_POINT ( 'NONE',  ( 0.5130740159365840825, 0.2530785775239950963, 0.9399606299212597271 ) ) ;
#19159 = EDGE_CURVE ( 'NONE', #16146, #16265, #25111, .T. ) ;
#19160 = ORIENTED_EDGE ( 'NONE', *, *, #13304, .T. ) ;
#19161 = ORIENTED_EDGE ( 'NONE', *, *, #16954, .T. ) ;
#19162 = ORIENTED_EDGE ( 'NONE', *, *, #9210, .F. ) ;
#19163 = ADVANCED_FACE ( 'NONE', ( #26260 ), #753, .T. ) ;
#19164 = CARTESIAN_POINT ( 'NONE',  ( 0.000000000000000000, 0.000000000000000000, 0.2637795275590551491 ) ) ;
#19165 = CARTESIAN_POINT ( 'NONE',  ( 0.5280699926562971713, -0.06957181182499251604, 1.747047244094488194 ) ) ;
#19166 = CARTESIAN_POINT ( 'NONE',  ( 0.4954415918530860607, 0.1327036767659604266, 1.766732283464566899 ) ) ;
#19167 = ADVANCED_FACE ( 'NONE', ( #23746, #4380 ), #24276, .T. ) ;
#19168 = AXIS2_PLACEMENT_3D ( 'NONE', #1936, #4335, #2074 ) ;
#19169 = ORIENTED_EDGE ( 'NONE', *, *, #15471, .F. ) ;
#19170 = ORIENTED_EDGE ( 'NONE', *, *, #8862, .T. ) ;
#19171 = CARTESIAN_POINT ( 'NONE',  ( -0.3574975638436101444, -0.02339816079122979120, -3.115157480314960647 ) ) ;
#19172 = ORIENTED_EDGE ( 'NONE', *, *, #9105, .T. ) ;
#19173 = EDGE_CURVE ( 'NONE', #12205, #15615, #15209, .T. ) ;
#19174 = CARTESIAN_POINT ( 'NONE',  ( 0.4688657571997049134, 0.08326155277540096822, 0.2330651858139422827 ) ) ;
#19175 = ORIENTED_EDGE ( 'NONE', *, *, #27839, .F. ) ;
#19176 = SHAPE_REPRESENTATION_RELATIONSHIP ( 'NONE' , 'NONE' ,  #27787, #18767 ) ;
#19177 = APPLICATION_CONTEXT ( 'automotive_design' ) ;
#19178 = CARTESIAN_POINT ( 'NONE',  ( 3.387491338582676492E-16, -0.6299212598425195653, 0.5915354330708662012 ) ) ;
#19179 = CARTESIAN_POINT ( 'NONE',  ( -0.1482986320106401412, 0.3007905576423888783, 1.973425196850393970 ) ) ;
#19180 = EDGE_LOOP ( 'NONE', ( #6771, #906 ) ) ;
#19181 = ORIENTED_EDGE ( 'NONE', *, *, #18189, .F. ) ;
#19182 = VECTOR ( 'NONE', #17298, 39.37007874015748143 ) ;
#19183 = CARTESIAN_POINT ( 'NONE',  ( 0.4270824798167662806, 0.2466292688014931900, -1.550196850393700920 ) ) ;
#19184 = AXIS2_PLACEMENT_3D ( 'NONE', #26142, #21907, #13550 ) ;
#19185 = EDGE_LOOP ( 'NONE', ( #5246, #14287, #7781, #24714, #15022 ) ) ;
#19186 = EDGE_LOOP ( 'NONE', ( #17771, #27731, #9019, #19109, #14635 ) ) ;
#19187 = ORIENTED_EDGE ( 'NONE', *, *, #26709, .F. ) ;
#19188 = CARTESIAN_POINT ( 'NONE',  ( -0.09842519685039370636, -5.111401574803149519E-18, 0.000000000000000000 ) ) ;
#19189 = PLANE ( 'NONE',  #12167 ) ;
#19190 = DIRECTION ( 'NONE',  ( 1.000000000000000000, 0.000000000000000000, 0.000000000000000000 ) ) ;
#19191 = DIRECTION ( 'NONE',  ( 0.000000000000000000, 0.000000000000000000, 1.000000000000000000 ) ) ;
#19192 = VERTEX_POINT ( 'NONE', #17894 ) ;
#19193 = AXIS2_PLACEMENT_3D ( 'NONE', #24750, #18235, #9630 ) ;
#19194 = CARTESIAN_POINT ( 'NONE',  ( 0.1493967478962657525, -0.2236290876712151154, -0.4249995598268396790 ) ) ;
#19195 = LINE ( 'NONE', #23599, #17733 ) ;
#19196 = CARTESIAN_POINT ( 'NONE',  ( -4.821283464566928349E-18, 0.000000000000000000, -0.2834645669291338543 ) ) ;
#19197 = DIRECTION ( 'NONE',  ( 0.000000000000000000, 0.000000000000000000, 1.000000000000000000 ) ) ;
#19199 = ADVANCED_FACE ( 'NONE', ( #26520 ), #24218, .F. ) ;
#19198 = AXIS2_PLACEMENT_3D ( 'NONE', #6981, #26586, #22081 ) ;
#19200 = CARTESIAN_POINT ( 'NONE',  ( -0.5350618161473178480, -0.4315538544190011261, 0.1618230966487632372 ) ) ;
#19201 = AXIS2_PLACEMENT_3D ( 'NONE', #22189, #26697, #726 ) ;
#19202 = CARTESIAN_POINT ( 'NONE',  ( 0.5393700787401575214, 0.000000000000000000, 0.2755905511811023723 ) ) ;
#19203 = DIRECTION ( 'NONE',  ( 1.000000000000000000, 0.000000000000000000, 0.000000000000000000 ) ) ;
#19204 = EDGE_CURVE ( 'NONE', #27489, #17779, #21232, .T. ) ;
#19205 = DIRECTION ( 'NONE',  ( -1.000000000000000000, 0.000000000000000000, 0.000000000000000000 ) ) ;
#19206 = CIRCLE ( 'NONE', #5221, 0.1181102362204718703 ) ;
#19207 = CARTESIAN_POINT ( 'NONE',  ( 0.09842519685039363697, 0.2165354330708661457, -3.259751644589254482 ) ) ;
#19208 = ORIENTED_EDGE ( 'NONE', *, *, #6448, .F. ) ;
#19209 = FACE_BOUND ( 'NONE', #7424, .T. ) ;
#19210 = DIRECTION ( 'NONE',  ( 0.000000000000000000, 0.000000000000000000, 1.000000000000000000 ) ) ;
#19211 = CIRCLE ( 'NONE', #16505, 0.07874015748031489015 ) ;
#19212 = ORIENTED_EDGE ( 'NONE', *, *, #3828, .F. ) ;
#19213 = CARTESIAN_POINT ( 'NONE',  ( 0.000000000000000000, 0.000000000000000000, -4.015748031496062964 ) ) ;
#19214 = CARTESIAN_POINT ( 'NONE',  ( -0.3759206409296168561, 0.2989751379763687655, 0.2362204724409447676 ) ) ;
#19215 = CARTESIAN_POINT ( 'NONE',  ( 0.5511811023622047445, -0.03607471876262466348, 0.9202755905511811330 ) ) ;
#19216 = EDGE_LOOP ( 'NONE', ( #18023, #5430 ) ) ;
#19217 = ORIENTED_EDGE ( 'NONE', *, *, #23660, .F. ) ;
#19218 = EDGE_CURVE ( 'NONE', #13130, #1165, #24649, .T. ) ;
#19219 = DIRECTION ( 'NONE',  ( -0.000000000000000000, 1.000000000000000000, -0.000000000000000000 ) ) ;
#19220 = CARTESIAN_POINT ( 'NONE',  ( 0.000000000000000000, 0.000000000000000000, 0.02362204724409448786 ) ) ;
#19221 = AXIS2_PLACEMENT_3D ( 'NONE', #26996, #3520, #24864 ) ;
#19222 = DIRECTION ( 'NONE',  ( -0.000000000000000000, -1.000000000000000000, -0.000000000000000000 ) ) ;
#19223 = DIRECTION ( 'NONE',  ( 0.000000000000000000, 0.000000000000000000, 1.000000000000000000 ) ) ;
#19224 = CARTESIAN_POINT ( 'NONE',  ( 0.000000000000000000, 0.07874015748031495954, -1.811023622047243542 ) ) ;
#19225 = AXIS2_PLACEMENT_3D ( 'NONE', #1322, #25044, #27450 ) ;
#19226 = ORIENTED_EDGE ( 'NONE', *, *, #26451, .T. ) ;
#19227 = CARTESIAN_POINT ( 'NONE',  ( 0.000000000000000000, 0.000000000000000000, 0.3425196850393700809 ) ) ;
#19228 = CARTESIAN_POINT ( 'NONE',  ( 0.5376957092749645728, -0.3112026930392428614, 0.09685039370078740717 ) ) ;
#19229 = CARTESIAN_POINT ( 'NONE',  ( 0.3346456692913385988, -0.02190250779246876237, 1.973425196850393970 ) ) ;
#19230 = CARTESIAN_POINT ( 'NONE',  ( 0.000000000000000000, 0.03937007874015751446, 0.000000000000000000 ) ) ;
#19231 = DIRECTION ( 'NONE',  ( 0.1736481776669301369, -0.9848077530122081313, 0.000000000000000000 ) ) ;
#19232 = DIRECTION ( 'NONE',  ( 0.000000000000000000, -1.000000000000000000, 0.000000000000000000 ) ) ;
#19233 = ADVANCED_FACE ( 'NONE', ( #4644 ), #10016, .T. ) ;
#19234 = CARTESIAN_POINT ( 'NONE',  ( 0.5230301363770953893, -0.1775991818008574585, 0.9399606299212598381 ) ) ;
#19235 = EDGE_CURVE ( 'NONE', #1325, #26728, #1842, .T. ) ;
#19236 = CYLINDRICAL_SURFACE ( 'NONE', #21394, 0.09842519685039378963 ) ;
#19237 = ORIENTED_EDGE ( 'NONE', *, *, #11979, .F. ) ;
#19238 = CARTESIAN_POINT ( 'NONE',  ( 0.1584824234590462289, 0.3213085410495249983, -3.115157480314959759 ) ) ;
#19239 = B_SPLINE_CURVE_WITH_KNOTS ( 'NONE', 3,
 ( #27156, #4121, #4263, #326, #10753, #3982 ),
 .UNSPECIFIED., .F., .F.,
 ( 4, 2, 4 ),
 ( 0.000000000000000000, 0.2500000000000000000, 0.5000000000000000000 ),
 .UNSPECIFIED. ) ;
#19240 = EDGE_CURVE ( 'NONE', #24509, #25577, #2827, .T. ) ;
#19242 = ORIENTED_EDGE ( 'NONE', *, *, #11446, .F. ) ;
#19243 = CIRCLE ( 'NONE', #16100, 0.1023622047244094474 ) ;
#19244 = ORIENTED_EDGE ( 'NONE', *, *, #24231, .F. ) ;
#19245 = TOROIDAL_SURFACE ( 'NONE', #13839, 0.4232283464566928832, 0.07677165354330708902 ) ;
#19246 = CARTESIAN_POINT ( 'NONE',  ( -0.4423390553432768879, -0.2180862235769457091, -1.550196850393700920 ) ) ;
#19247 = CARTESIAN_POINT ( 'NONE',  ( 0.5525858403826197085, -0.1481194149833565954, 0.9399606299212598381 ) ) ;
#19248 = CYLINDRICAL_SURFACE ( 'NONE', #17512, 0.6881889763779527325 ) ;
#19249 = FACE_BOUND ( 'NONE', #9184, .T. ) ;
#19250 = DIRECTION ( 'NONE',  ( 0.000000000000000000, 0.000000000000000000, 1.000000000000000000 ) ) ;
#19251 = DIRECTION ( 'NONE',  ( 0.000000000000000000, 0.000000000000000000, 1.000000000000000000 ) ) ;
#19252 = EDGE_LOOP ( 'NONE', ( #14255, #9995, #5273, #7503 ) ) ;
#19253 = DIRECTION ( 'NONE',  ( 0.000000000000000000, 0.000000000000000000, 1.000000000000000000 ) ) ;
#19254 = DIRECTION ( 'NONE',  ( 0.7071067818211370648, -0.7071067805519580807, 0.000000000000000000 ) ) ;
#19255 = DIRECTION ( 'NONE',  ( 0.000000000000000000, 0.000000000000000000, 1.000000000000000000 ) ) ;
#19256 = DIRECTION ( 'NONE',  ( 0.000000000000000000, 0.000000000000000000, 1.000000000000000000 ) ) ;
#19257 = ORIENTED_EDGE ( 'NONE', *, *, #3329, .F. ) ;
#19258 = CARTESIAN_POINT ( 'NONE',  ( -0.4338922498494567348, -0.2500511477696472085, 0.2574819596263889787 ) ) ;
#19259 = DIRECTION ( 'NONE',  ( -0.7818314824680298036, 0.6234898018587337054, 0.000000000000000000 ) ) ;
#19260 = CARTESIAN_POINT ( 'NONE',  ( -0.2228021814315760130, -0.4641672719513419976, 0.1473214333387365127 ) ) ;
#19261 = ORIENTED_EDGE ( 'NONE', *, *, #11700, .F. ) ;
#19262 = CARTESIAN_POINT ( 'NONE',  ( -0.4327133464953751840, -0.2505177833316183933, 0.1259302777263945627 ) ) ;
#19263 = CARTESIAN_POINT ( 'NONE',  ( 0.1275996891957731083, 0.4763861460130595082, -1.550196850393700920 ) ) ;
#19264 = CARTESIAN_POINT ( 'NONE',  ( -0.4382752542995838052, -0.1173917140416377847, -1.934055118110236338 ) ) ;
#19265 = AXIS2_PLACEMENT_3D ( 'NONE', #10678, #23695, #8667 ) ;
#19266 = AXIS2_PLACEMENT_3D ( 'NONE', #4031, #14217, #1347 ) ;
#19267 = EDGE_CURVE ( 'NONE', #12544, #17596, #14603, .T. ) ;
#19268 = CARTESIAN_POINT ( 'NONE',  ( -2.185478346456693112E-16, 0.6299212598071869396, -7.714310545377398371E-17 ) ) ;
#19269 = EDGE_CURVE ( 'NONE', #25742, #11937, #1016, .T. ) ;
#19270 = ORIENTED_EDGE ( 'NONE', *, *, #25719, .T. ) ;
#19271 = CARTESIAN_POINT ( 'NONE',  ( -0.4769977115679039370, -0.4103508094347110280, -0.3464985434502441120 ) ) ;
#19272 = DIRECTION ( 'NONE',  ( 0.000000000000000000, 1.000000000000000000, 0.000000000000000000 ) ) ;
#19273 = CARTESIAN_POINT ( 'NONE',  ( 0.5314960629921260393, 0.000000000000000000, 1.747047244094488194 ) ) ;
#19274 = FILL_AREA_STYLE_COLOUR ( '', #12531 ) ;
#19275 = ( BOUNDED_CURVE ( )  B_SPLINE_CURVE ( 2, ( #5340, #26958, #24678 ),
 .UNSPECIFIED., .F., .T. ) 
 B_SPLINE_CURVE_WITH_KNOTS ( ( 3, 3 ),
 ( 0.1168436138077912356, 0.2336872276155829986 ),
 .UNSPECIFIED. ) 
 CURVE ( )  GEOMETRIC_REPRESENTATION_ITEM ( )  RATIONAL_B_SPLINE_CURVE ( ( 1.077350269189625953, 1.077350269189626175, 1.000000000000000000 ) ) 
 REPRESENTATION_ITEM ( '' )  ) ;
#19276 = CARTESIAN_POINT ( 'NONE',  ( -0.1771653543307086520, 0.6299212598425196763, 0.000000000000000000 ) ) ;
#19277 = CARTESIAN_POINT ( 'NONE',  ( -0.6064063350436810218, -0.5142385541152183492, 0.9905098495108229928 ) ) ;
#19278 = ( GEOMETRIC_REPRESENTATION_CONTEXT ( 3 ) GLOBAL_UNCERTAINTY_ASSIGNED_CONTEXT ( ( #27126 ) ) GLOBAL_UNIT_ASSIGNED_CONTEXT ( ( #27106, #5493, #22870 ) ) REPRESENTATION_CONTEXT ( 'NONE', 'WORKASPACE' ) ) ;
#19279 = DIRECTION ( 'NONE',  ( 0.000000000000000000, 0.000000000000000000, 1.000000000000000000 ) ) ;
#19280 = PRODUCT ( 'Tapered Roller Bearing 17x40x17', 'Tapered Roller Bearing 17x40x17', '', ( #7554 ) ) ;
#19281 = CARTESIAN_POINT ( 'NONE',  ( -0.1153552079393971586, 0.4303653410901769893, -1.934055118110237004 ) ) ;
#19282 = ORIENTED_EDGE ( 'NONE', *, *, #21913, .T. ) ;
#19283 = CARTESIAN_POINT ( 'NONE',  ( 0.2817310484609266696, -0.2161381151962942504, 1.953740157480315043 ) ) ;
#19284 = ORIENTED_EDGE ( 'NONE', *, *, #7598, .T. ) ;
#19285 = CARTESIAN_POINT ( 'NONE',  ( -0.5930505946656516869, -0.1422258853902071407, -0.2487018284346101948 ) ) ;
#19286 = CARTESIAN_POINT ( 'NONE',  ( 0.8031496062992127261, 0.000000000000000000, 0.4724409448818898127 ) ) ;
#19287 = CARTESIAN_POINT ( 'NONE',  ( -0.3772436174784659646, -0.4300830224589956563, 0.9399606299212598381 ) ) ;
#19288 = CARTESIAN_POINT ( 'NONE',  ( 0.1532705055535415473, -0.6139925424104980545, -0.2937959843914932923 ) ) ;
#19289 = DIRECTION ( 'NONE',  ( 0.000000000000000000, 1.000000000000000000, 0.000000000000000000 ) ) ;
#19290 = EDGE_CURVE ( 'NONE', #5023, #14218, #4293, .T. ) ;
#19291 = CARTESIAN_POINT ( 'NONE',  ( -0.1867299569291685502, -0.3233561589689051829, -3.115157480314960647 ) ) ;
#19292 = CARTESIAN_POINT ( 'NONE',  ( -0.08600259727896251982, 0.2165354330708660902, -3.597797143737292203 ) ) ;
#19293 = CARTESIAN_POINT ( 'NONE',  ( 0.2395669291338582696, 2.933848729453403498E-17, 0.000000000000000000 ) ) ;
#19294 = DIRECTION ( 'NONE',  ( 0.000000000000000000, 0.000000000000000000, -1.000000000000000000 ) ) ;
#19295 = FACE_OUTER_BOUND ( 'NONE', #5420, .T. ) ;
#19296 = CARTESIAN_POINT ( 'NONE',  ( 0.0005896702191646874128, 0.4865884552430826959, 0.09284957166429574915 ) ) ;
#19297 = EDGE_CURVE ( 'NONE', #23414, #27631, #27851, .T. ) ;
#19298 = AXIS2_PLACEMENT_3D ( 'NONE', #22891, #861, #11720 ) ;
#19299 = TOROIDAL_SURFACE ( 'NONE', #16159, 0.3740157480314960647, 0.03937007874015747977 ) ;
#19300 = ORIENTED_EDGE ( 'NONE', *, *, #11931, .F. ) ;
#19301 = CARTESIAN_POINT ( 'NONE',  ( -0.2395669291338582696, 0.000000000000000000, 0.000000000000000000 ) ) ;
#19302 = EDGE_LOOP ( 'NONE', ( #22684, #25305 ) ) ;
#19303 = EDGE_LOOP ( 'NONE', ( #9607, #8588, #19585, #9459 ) ) ;
#19304 = CARTESIAN_POINT ( 'NONE',  ( 0.000000000000000000, 0.000000000000000000, -0.1756889763779527769 ) ) ;
#19305 = EDGE_LOOP ( 'NONE', ( #3884, #12409 ) ) ;
#19306 = FACE_OUTER_BOUND ( 'NONE', #26683, .T. ) ;
#19307 = DIRECTION ( 'NONE',  ( 0.000000000000000000, 0.000000000000000000, -1.000000000000000000 ) ) ;
#19308 = CARTESIAN_POINT ( 'NONE',  ( -0.2268096725222462362, 0.4600326175560554565, 1.766732283464566899 ) ) ;
#19309 = CARTESIAN_POINT ( 'NONE',  ( -0.2268096725222397969, 0.4600326175560398023, 1.747047244094488194 ) ) ;
#19310 = DIRECTION ( 'NONE',  ( 1.000000000000000000, 0.000000000000000000, 0.000000000000000000 ) ) ;
#19311 = ORIENTED_EDGE ( 'NONE', *, *, #15237, .F. ) ;
#19312 = CARTESIAN_POINT ( 'NONE',  ( 0.3102476824511487541, -0.1791601451668820011, -3.115157480314960647 ) ) ;
#19313 = ORIENTED_EDGE ( 'NONE', *, *, #9757, .F. ) ;
#19314 = CARTESIAN_POINT ( 'NONE',  ( -0.1704479274139978628, -0.4700505334955267234, 0.1496602734641385990 ) ) ;
#19315 = LENGTH_MEASURE_WITH_UNIT ( LENGTH_MEASURE( 0.02539999999999999897 ), #14831 ) ;
#19316 = LINE ( 'NONE', #1944, #4600 ) ;
#19317 = CIRCLE ( 'NONE', #15263, 0.3771653543307086909 ) ;
#19318 = CARTESIAN_POINT ( 'NONE',  ( 0.1078280746904042159, 0.3175540113612283499, 1.973425196850393970 ) ) ;
#19319 = EDGE_LOOP ( 'NONE', ( #1043, #24239 ) ) ;
#19320 = VERTEX_POINT ( 'NONE', #2835 ) ;
#19321 = AXIS2_PLACEMENT_3D ( 'NONE', #16000, #7518, #7105 ) ;
#19322 = ORIENTED_EDGE ( 'NONE', *, *, #27699, .T. ) ;
#19323 = ( GEOMETRIC_REPRESENTATION_CONTEXT ( 3 ) GLOBAL_UNCERTAINTY_ASSIGNED_CONTEXT ( ( #5651 ) ) GLOBAL_UNIT_ASSIGNED_CONTEXT ( ( #224, #6827, #21797 ) ) REPRESENTATION_CONTEXT ( 'NONE', 'WORKASPACE' ) ) ;
#19324 = ORIENTED_EDGE ( 'NONE', *, *, #12248, .T. ) ;
#19325 = ORIENTED_EDGE ( 'NONE', *, *, #14418, .T. ) ;
#19326 = ORIENTED_EDGE ( 'NONE', *, *, #3202, .T. ) ;
#19327 = CARTESIAN_POINT ( 'NONE',  ( 0.4898768902087983768, 0.000000000000000000, -0.2362204724409449064 ) ) ;
#19328 = EDGE_CURVE ( 'NONE', #7057, #21158, #15661, .T. ) ;
#19329 = DIRECTION ( 'NONE',  ( 0.000000000000000000, 0.000000000000000000, -1.000000000000000000 ) ) ;
#19330 = CARTESIAN_POINT ( 'NONE',  ( 0.000000000000000000, 0.000000000000000000, -0.01377952755905511792 ) ) ;
#19331 = B_SPLINE_CURVE_WITH_KNOTS ( 'NONE', 3,
 ( #16632, #27232, #27096, #25247, #7744, #24960 ),
 .UNSPECIFIED., .F., .F.,
 ( 4, 2, 4 ),
 ( 0.2291966065698859967, 0.2305109203526899964, 0.2318252341354939960 ),
 .UNSPECIFIED. ) ;
#19332 = CARTESIAN_POINT ( 'NONE',  ( 0.4015002836602225567, -0.2311469024248521409, 0.2048502514551664710 ) ) ;
#19333 = ORIENTED_EDGE ( 'NONE', *, *, #7653, .F. ) ;
#19334 = EDGE_CURVE ( 'NONE', #7273, #25216, #10693, .T. ) ;
#19335 = B_SPLINE_CURVE_WITH_KNOTS ( 'NONE', 3,
 ( #26033, #4819, #4288, #2691, #12894, #15037 ),
 .UNSPECIFIED., .F., .F.,
 ( 4, 2, 4 ),
 ( 0.5000000000000000000, 0.7500000000000000000, 1.000000000000000000 ),
 .UNSPECIFIED. ) ;
#19336 = CARTESIAN_POINT ( 'NONE',  ( 0.3002886982018046491, -0.1727973894384566000, 0.1377952755905509363 ) ) ;
#19337 = ITEM_DEFINED_TRANSFORMATION ( 'NONE', 'NONE', #25143,  #11588 ) ;
#19338 = EDGE_CURVE ( 'NONE', #8838, #18929, #11100, .T. ) ;
#19339 = CIRCLE ( 'NONE', #15311, 0.07677362204724409722 ) ;
#19340 = FACE_OUTER_BOUND ( 'NONE', #9149, .T. ) ;
#19341 = CARTESIAN_POINT ( 'NONE',  ( -0.4620608682196457040, 0.08206165078054665496, 0.07637795275590551769 ) ) ;
#19342 = AXIS2_PLACEMENT_3D ( 'NONE', #16253, #12010, #11861 ) ;
#19343 = CARTESIAN_POINT ( 'NONE',  ( -0.6299212598425196763, 1.087444635826771533, 0.1051828227901515783 ) ) ;
#19344 = CARTESIAN_POINT ( 'NONE',  ( -0.09842519685039370636, 0.07874015748031495954, -0.04546065111729338803 ) ) ;
#19345 = B_SPLINE_CURVE_WITH_KNOTS ( 'NONE', 3,
 ( #18334, #854, #994, #26536, #11575, #5214 ),
 .UNSPECIFIED., .F., .F.,
 ( 4, 2, 4 ),
 ( 0.5000000000000000000, 0.7500000000000000000, 1.000000000000000000 ),
 .UNSPECIFIED. ) ;
#19346 = CARTESIAN_POINT ( 'NONE',  ( 0.06048688226688470060, 0.1968503937007873850, -3.193930429277340277 ) ) ;
#19347 = ORIENTED_EDGE ( 'NONE', *, *, #209, .F. ) ;
#19348 = AXIS2_PLACEMENT_3D ( 'NONE', #2191, #11089, #117 ) ;
#19349 = ORIENTED_EDGE ( 'NONE', *, *, #2073, .F. ) ;
#19350 = CARTESIAN_POINT ( 'NONE',  ( -0.09842519685039370636, 0.07874015748031495954, 0.04546065111729331171 ) ) ;
#19351 = CARTESIAN_POINT ( 'NONE',  ( 0.1293227632562456708, -0.3543012242648960752, 0.07637630750536809898 ) ) ;
#19352 = ORIENTED_EDGE ( 'NONE', *, *, #18637, .T. ) ;
#19353 = ORIENTED_EDGE ( 'NONE', *, *, #20623, .F. ) ;
#19354 = CARTESIAN_POINT ( 'NONE',  ( -0.5816225468157798506, 1.097802432538817152, -0.08994119036359567165 ) ) ;
#19355 = CARTESIAN_POINT ( 'NONE',  ( -0.03532354024591901481, -0.8267716535433071723, 0.000000000000000000 ) ) ;
#19356 = B_SPLINE_CURVE_WITH_KNOTS ( 'NONE', 3,
 ( #19869, #21719, #11248, #21581, #9115, #26224 ),
 .UNSPECIFIED., .F., .F.,
 ( 4, 2, 4 ),
 ( 1.217380381967464009, 1.219305002860850085, 1.221229623754231941 ),
 .UNSPECIFIED. ) ;
#19357 = CARTESIAN_POINT ( 'NONE',  ( -0.4783323773986509764, -0.2762247810519017355, 0.9202755905511811330 ) ) ;
#19358 = ORIENTED_EDGE ( 'NONE', *, *, #27124, .T. ) ;
#19359 = DIRECTION ( 'NONE',  ( 0.000000000000000000, 0.000000000000000000, 1.000000000000000000 ) ) ;
#19360 = ORIENTED_EDGE ( 'NONE', *, *, #25196, .T. ) ;
#19361 = EDGE_CURVE ( 'NONE', #14467, #17381, #19206, .T. ) ;
#19362 = CARTESIAN_POINT ( 'NONE',  ( 0.3002886982018046491, -0.1727973894384566000, 0.1377952755905509363 ) ) ;
#19363 = CARTESIAN_POINT ( 'NONE',  ( 0.2358179517425398330, 0.2802411498256521249, 0.1910323752979251055 ) ) ;
#19364 = CIRCLE ( 'NONE', #9878, 0.5322834645669292097 ) ;
#19365 = CARTESIAN_POINT ( 'NONE',  ( -1.197070535079588716, 0.07874015748031491790, -1.315180771300060503 ) ) ;
#19366 = CARTESIAN_POINT ( 'NONE',  ( 0.000000000000000000, 0.5322834645669292097, 0.4062992125984251635 ) ) ;
#19367 = DIRECTION ( 'NONE',  ( 0.6427876096865398070, 0.7660444431189775694, -0.000000000000000000 ) ) ;
#19368 = EDGE_CURVE ( 'NONE', #4739, #5673, #22364, .T. ) ;
#19369 = ORIENTED_EDGE ( 'NONE', *, *, #17183, .F. ) ;
#19370 = CARTESIAN_POINT ( 'NONE',  ( -1.928577543407793639E-16, 0.07874015748031495954, 1.811023622047243542 ) ) ;
#19371 = CARTESIAN_POINT ( 'NONE',  ( -0.5905511811023621549, -0.4724409448818898127, -0.8182917201112815953 ) ) ;
#19372 = CIRCLE ( 'NONE', #22060, 0.1082677165354330312 ) ;
#19373 = CARTESIAN_POINT ( 'NONE',  ( -0.4771018889076559244, 0.3804760601893846794, 0.1062972440944881941 ) ) ;
#19374 = CARTESIAN_POINT ( 'NONE',  ( 0.2420394123212937232, 0.2892587550802425134, 0.1992125984251968684 ) ) ;
#19375 = CARTESIAN_POINT ( 'NONE',  ( 0.000000000000000000, 0.000000000000000000, -0.3779527559055118058 ) ) ;
#19376 = EDGE_CURVE ( 'NONE', #20990, #25275, #18861, .T. ) ;
#19377 = FACE_OUTER_BOUND ( 'NONE', #18390, .T. ) ;
#19378 = ORIENTED_EDGE ( 'NONE', *, *, #296, .T. ) ;
#19379 = CARTESIAN_POINT ( 'NONE',  ( 0.02345921195965492909, 0.3574989824755535617, -3.115157480314959759 ) ) ;
#19380 = CONICAL_SURFACE ( 'NONE', #17566, 0.4527559054764771496, 0.7853981642949022790 ) ;
#19381 = ADVANCED_FACE ( 'NONE', ( #23137 ), #11991, .F. ) ;
#19382 = AXIS2_PLACEMENT_3D ( 'NONE', #12659, #27511, #8154 ) ;
#19383 = ORIENTED_EDGE ( 'NONE', *, *, #26481, .T. ) ;
#19384 = VERTEX_POINT ( 'NONE', #16487 ) ;
#19385 = ORIENTED_EDGE ( 'NONE', *, *, #4766, .F. ) ;
#19386 = CARTESIAN_POINT ( 'NONE',  ( -0.3121994997578197428, 0.4069448477569481692, -1.550196850393700920 ) ) ;
#19387 = FACE_OUTER_BOUND ( 'NONE', #25824, .T. ) ;
#19388 = FACE_OUTER_BOUND ( 'NONE', #15908, .T. ) ;
#19389 = DIRECTION ( 'NONE',  ( 0.000000000000000000, -0.000000000000000000, -1.000000000000000000 ) ) ;
#19390 = DIRECTION ( 'NONE',  ( -1.224646799147353207E-16, 1.000000000000000000, 0.000000000000000000 ) ) ;
#19391 = ORIENTED_EDGE ( 'NONE', *, *, #15524, .T. ) ;
#19392 = CARTESIAN_POINT ( 'NONE',  ( -0.2997912780622379314, -0.1736589463928940036, 0.1478915661223339784 ) ) ;
#19393 = ORIENTED_EDGE ( 'NONE', *, *, #20021, .F. ) ;
#19394 = ORIENTED_EDGE ( 'NONE', *, *, #10067, .T. ) ;
#19395 = EDGE_CURVE ( 'NONE', #27334, #24760, #18757, .T. ) ;
#19396 = CARTESIAN_POINT ( 'NONE',  ( -0.4901574803149605919, 0.000000000000000000, -6.034492125984251821E-17 ) ) ;
#19397 = ADVANCED_FACE ( 'NONE', ( #25103 ), #25244, .T. ) ;
#19398 = DIRECTION ( 'NONE',  ( 0.000000000000000000, 0.000000000000000000, 1.000000000000000000 ) ) ;
#19399 = DIRECTION ( 'NONE',  ( 1.000000000000000000, 0.000000000000000000, 0.000000000000000000 ) ) ;
#19400 = ADVANCED_FACE ( 'NONE', ( #3770, #14680 ), #7594, .T. ) ;
#19401 = CIRCLE ( 'NONE', #2246, 0.5905511811023621549 ) ;
#19402 = AXIS2_PLACEMENT_3D ( 'NONE', #20755, #7904, #25410 ) ;
#19403 = FACE_OUTER_BOUND ( 'NONE', #1069, .T. ) ;
#19404 = VERTEX_POINT ( 'NONE', #26949 ) ;
#19405 = DIRECTION ( 'NONE',  ( 0.000000000000000000, 0.000000000000000000, 1.000000000000000000 ) ) ;
#19406 = CARTESIAN_POINT ( 'NONE',  ( -0.3912931228432124930, 0.3001918266902225407, -1.550196850393700920 ) ) ;
#19407 = ADVANCED_FACE ( 'NONE', ( #27291 ), #11986, .T. ) ;
#19408 = CARTESIAN_POINT ( 'NONE',  ( 0.3411003281197156900, -0.2991932138496291582, -1.934055118110236338 ) ) ;
#19409 = EDGE_CURVE ( 'NONE', #20656, #21760, #10767, .T. ) ;
#19410 = DIRECTION ( 'NONE',  ( 3.508908000000000588E-18, -0.4999999999999998890, -0.8660254037844388186 ) ) ;
#19411 = CARTESIAN_POINT ( 'NONE',  ( 0.000000000000000000, 0.000000000000000000, 0.2574803149606298969 ) ) ;
#19412 = CARTESIAN_POINT ( 'NONE',  ( -0.5501272682971083405, 0.4396946356847500903, 0.1443310008616609796 ) ) ;
#19413 = ORIENTED_EDGE ( 'NONE', *, *, #23798, .T. ) ;
#19414 = CARTESIAN_POINT ( 'NONE',  ( -0.4995226175161708859, -0.3565589576102653480, -0.3180767762144185440 ) ) ;
#19415 = CARTESIAN_POINT ( 'NONE',  ( 0.1638952246732497953, 0.2749627978706437048, 0.4762495361032464958 ) ) ;
#19416 = CARTESIAN_POINT ( 'NONE',  ( 0.1506723201675407575, 0.000000000000000000, 0.000000000000000000 ) ) ;
#19417 = CIRCLE ( 'NONE', #14947, 0.4986013261500205074 ) ;
#19418 = CARTESIAN_POINT ( 'NONE',  ( -0.1601448837025507554, -0.4411213145380000200, 0.07637630773773071424 ) ) ;
#19419 = B_SPLINE_CURVE_WITH_KNOTS ( 'NONE', 2,
 ( #8254, #11674, #18144 ),
 .UNSPECIFIED., .F., .F.,
 ( 3, 3 ),
 ( 0.000000000000000000, 1.000000000000000000 ),
 .UNSPECIFIED. ) ;
#19420 = CARTESIAN_POINT ( 'NONE',  ( -0.09842519685039370636, 0.1673228346456692994, 0.000000000000000000 ) ) ;
#19421 = CARTESIAN_POINT ( 'NONE',  ( 0.2173565190923199553, -0.5952284643130145714, 0.1061598535646071789 ) ) ;
#19422 = ORIENTED_EDGE ( 'NONE', *, *, #5522, .F. ) ;
#19423 = CARTESIAN_POINT ( 'NONE',  ( -0.6806799598997224088, 0.06756148199031772328, -0.08096199836402361016 ) ) ;
#19424 = ORIENTED_EDGE ( 'NONE', *, *, #21013, .F. ) ;
#19425 = ADVANCED_FACE ( 'NONE', ( #21020 ), #6431, .T. ) ;
#19426 = CARTESIAN_POINT ( 'NONE',  ( -0.3858397471888894703, -0.2228126397719936702, -1.934055118110236338 ) ) ;
#19427 = AXIS2_PLACEMENT_3D ( 'NONE', #10055, #25035, #18234 ) ;
#19428 = CYLINDRICAL_SURFACE ( 'NONE', #6272, 0.6881889763779527325 ) ;
#19429 = CARTESIAN_POINT ( 'NONE',  ( -0.6869867706933208140, 0.6386884284781711996, -0.3000169784712433119 ) ) ;
#19430 = ADVANCED_FACE ( 'NONE', ( #1350 ), #8389, .F. ) ;
#19431 = ADVANCED_FACE ( 'NONE', ( #9959 ), #12084, .T. ) ;
#19432 = CARTESIAN_POINT ( 'NONE',  ( 0.6299212598425196763, 0.04921259842519685318, 0.000000000000000000 ) ) ;
#19433 = CARTESIAN_POINT ( 'NONE',  ( 0.3349073414797994475, -0.1651192144506243853, -3.115157480314960647 ) ) ;
#19434 = DIRECTION ( 'NONE',  ( 0.000000000000000000, 0.000000000000000000, -1.000000000000000000 ) ) ;
#19435 = CARTESIAN_POINT ( 'NONE',  ( 0.3937007874015748254, 0.03937007874015750059, 0.000000000000000000 ) ) ;
#19436 = CARTESIAN_POINT ( 'NONE',  ( 0.000000000000000000, 0.5610236220472440971, 0.1771653543307086520 ) ) ;
#19437 = CIRCLE ( 'NONE', #2290, 0.5007874015748031704 ) ;
#19438 = ORIENTED_EDGE ( 'NONE', *, *, #25037, .T. ) ;
#19439 = DIRECTION ( 'NONE',  ( 0.000000000000000000, 1.000000000000000000, 0.000000000000000000 ) ) ;
#19440 = ( BOUNDED_CURVE ( )  B_SPLINE_CURVE ( 3, ( #20636, #25150, #1288, #10309 ),
 .UNSPECIFIED., .F., .F. ) 
 B_SPLINE_CURVE_WITH_KNOTS ( ( 4, 4 ),
 ( 6.170019055269735375, 6.283185307179586232 ),
 .UNSPECIFIED. ) 
 CURVE ( )  GEOMETRIC_REPRESENTATION_ITEM ( )  RATIONAL_B_SPLINE_CURVE ( ( 1.000000000000000000, 0.9989330679932157953, 0.9989330679932157953, 1.000000000000000000 ) ) 
 REPRESENTATION_ITEM ( '' )  ) ;
#19441 = VECTOR ( 'NONE', #16926, 39.37007874015748854 ) ;
#19442 = ORIENTED_EDGE ( 'NONE', *, *, #24754, .T. ) ;
#19443 = ORIENTED_EDGE ( 'NONE', *, *, #26237, .T. ) ;
#19444 = CARTESIAN_POINT ( 'NONE',  ( 0.000000000000000000, 0.000000000000000000, 0.1992125984251968684 ) ) ;
#19445 = DIRECTION ( 'NONE',  ( 0.000000000000000000, 1.000000000000000000, 0.000000000000000000 ) ) ;
#19446 = DIRECTION ( 'NONE',  ( 0.000000000000000000, 0.000000000000000000, 1.000000000000000000 ) ) ;
#19447 = CARTESIAN_POINT ( 'NONE',  ( -0.2564944395515793563, -0.4441657790107725323, 1.747047244094488194 ) ) ;
#19448 = LINE ( 'NONE', #2079, #18066 ) ;
#19449 = ORIENTED_EDGE ( 'NONE', *, *, #13543, .T. ) ;
#19450 = ORIENTED_EDGE ( 'NONE', *, *, #25880, .F. ) ;
#19452 = CARTESIAN_POINT ( 'NONE',  ( -0.3726024258163779246, 0.000000000000000000, -3.115157480314960647 ) ) ;
#19451 = CARTESIAN_POINT ( 'NONE',  ( -0.1771653543307086520, -0.1673228346456692994, 2.049113738730807629E-17 ) ) ;
#19453 = VERTEX_POINT ( 'NONE', #22257 ) ;
#19454 = VERTEX_POINT ( 'NONE', #20568 ) ;
#19455 = DIRECTION ( 'NONE',  ( 1.000000000000000000, 0.000000000000000000, 0.000000000000000000 ) ) ;
#19456 = CARTESIAN_POINT ( 'NONE',  ( 0.3339160553493882300, 1.241955529277657622, -0.7081600496628897012 ) ) ;
#19457 = CARTESIAN_POINT ( 'NONE',  ( -0.2660793235464189999, 0.2041304421298406335, 1.953740157480315043 ) ) ;
#19458 = VERTEX_POINT ( 'NONE', #5593 ) ;
#19459 = ORIENTED_EDGE ( 'NONE', *, *, #9171, .F. ) ;
#19460 = CIRCLE ( 'NONE', #10439, 0.09842519685039370636 ) ;
#19461 = DIRECTION ( 'NONE',  ( 0.000000000000000000, 0.000000000000000000, 1.000000000000000000 ) ) ;
#19462 = ORIENTED_EDGE ( 'NONE', *, *, #24717, .T. ) ;
#19463 = VERTEX_POINT ( 'NONE', #17990 ) ;
#19464 = VERTEX_POINT ( 'NONE', #16329 ) ;
#19465 = CARTESIAN_POINT ( 'NONE',  ( -0.1706130639253582437, -0.4670119966449340909, 0.1615162260892915869 ) ) ;
#19466 = ADVANCED_FACE ( 'NONE', ( #9679 ), #20555, .F. ) ;
#19467 = VECTOR ( 'NONE', #18701, 39.37007874015748143 ) ;
#19468 = CARTESIAN_POINT ( 'NONE',  ( 0.000000000000000000, 0.000000000000000000, 0.09685039370078740717 ) ) ;
#19469 = DIRECTION ( 'NONE',  ( 0.000000000000000000, 0.000000000000000000, 1.000000000000000000 ) ) ;
#19470 = CARTESIAN_POINT ( 'NONE',  ( 0.3992017438595157897, -0.2298214351608010297, 0.1903859677804414230 ) ) ;
#19471 = CARTESIAN_POINT ( 'NONE',  ( -0.4613022222206683010, 0.2662775206743746015, 1.747047244094488416 ) ) ;
#19472 = CARTESIAN_POINT ( 'NONE',  ( -0.2952755905511810774, 0.000000000000000000, -0.07578740157480315376 ) ) ;
#19473 = CARTESIAN_POINT ( 'NONE',  ( -0.1570092758121678089, -0.4330450457732858416, 0.1771653543307084855 ) ) ;
#19474 = AXIS2_PLACEMENT_3D ( 'NONE', #12895, #92, #6686 ) ;
#19475 = CARTESIAN_POINT ( 'NONE',  ( -0.6010422146565906898, 1.121275077793808528, 0.01914631898548286096 ) ) ;
#19476 = DIRECTION ( 'NONE',  ( 0.000000000000000000, -1.000000000000000000, 0.000000000000000000 ) ) ;
#19477 = ADVANCED_FACE ( 'NONE', ( #1083 ), #10627, .T. ) ;
#19478 = EDGE_CURVE ( 'NONE', #19320, #1582, #1616, .T. ) ;
#19479 = CIRCLE ( 'NONE', #17229, 0.3771653543307086909 ) ;
#19480 = CARTESIAN_POINT ( 'NONE',  ( -0.06048688226689052927, 0.2165354330708661457, -3.193930429277413108 ) ) ;
#19481 = ORIENTED_EDGE ( 'NONE', *, *, #18641, .F. ) ;
#19482 = PRODUCT_DEFINITION ( 'UNKNOWN', '', #12983, #9944 ) ;
#19483 = DIRECTION ( 'NONE',  ( 0.000000000000000000, 0.000000000000000000, 1.000000000000000000 ) ) ;
#19484 = EDGE_CURVE ( 'NONE', #21760, #23475, #341, .T. ) ;
#19485 = LINE ( 'NONE', #7049, #2382 ) ;
#19486 = ORIENTED_EDGE ( 'NONE', *, *, #4823, .T. ) ;
#19487 = DIRECTION ( 'NONE',  ( 0.000000000000000000, 0.8660254037844385966, -0.4999999999999998335 ) ) ;
#19488 = CARTESIAN_POINT ( 'NONE',  ( -0.5694559772926249819, 1.112071903501507641, -0.05864771439935212438 ) ) ;
#19489 = EDGE_CURVE ( 'NONE', #22369, #16929, #22573, .T. ) ;
#19490 = CARTESIAN_POINT ( 'NONE',  ( 0.0007756954652683944150, 0.7174612052770362736, 0.1601585119462015649 ) ) ;
#19491 = EDGE_LOOP ( 'NONE', ( #15875, #15387, #412, #1115 ) ) ;
#19492 = CARTESIAN_POINT ( 'NONE',  ( -0.4954197419817713000, -0.2442565704126117565, 0.9202755905511811330 ) ) ;
#19493 = VERTEX_POINT ( 'NONE', #24645 ) ;
#19494 = DIRECTION ( 'NONE',  ( 0.000000000000000000, 0.000000000000000000, 1.000000000000000000 ) ) ;
#19495 = ORIENTED_EDGE ( 'NONE', *, *, #5071, .T. ) ;
#19496 = TOROIDAL_SURFACE ( 'NONE', #6875, 0.4232283464566928832, 0.07677165354330708902 ) ;
#19497 = CYLINDRICAL_SURFACE ( 'NONE', #12937, 0.4330708661417322913 ) ;
#19498 = ( LENGTH_UNIT ( ) NAMED_UNIT ( * ) SI_UNIT ( $, .METRE. ) ) ;
#19499 = AXIS2_PLACEMENT_3D ( 'NONE', #22037, #21906, #2798 ) ;
#19500 = CARTESIAN_POINT ( 'NONE',  ( 0.000000000000000000, 0.4724409448818898127, 0.000000000000000000 ) ) ;
#19501 = DIRECTION ( 'NONE',  ( 0.000000000000000000, 0.000000000000000000, 1.000000000000000000 ) ) ;
#19502 = ORIENTED_EDGE ( 'NONE', *, *, #21044, .T. ) ;
#19503 = CARTESIAN_POINT ( 'NONE',  ( 0.000000000000000000, 0.000000000000000000, -0.1377952755696461029 ) ) ;
#19504 = DIRECTION ( 'NONE',  ( 0.000000000000000000, 0.000000000000000000, 1.000000000000000000 ) ) ;
#19505 = CIRCLE ( 'NONE', #23127, 0.1003956692913385851 ) ;
#19506 = DIRECTION ( 'NONE',  ( 0.000000000000000000, 0.000000000000000000, 1.000000000000000000 ) ) ;
#19507 = CARTESIAN_POINT ( 'NONE',  ( 0.2223167940359795647, 0.2657206863494897542, 0.1377952755905510474 ) ) ;
#19508 = CARTESIAN_POINT ( 'NONE',  ( 0.4622619257814346572, 0.08092139668567618904, 0.07637795275590551769 ) ) ;
#19509 = CARTESIAN_POINT ( 'NONE',  ( -0.2427018018350767803, 0.2887032559529634224, 0.07637630750536809898 ) ) ;
#19510 = CARTESIAN_POINT ( 'NONE',  ( -7.608238775805210269E-17, -0.6212598425196850238, 0.3543307086614173040 ) ) ;
#19511 = AXIS2_PLACEMENT_3D ( 'NONE', #23124, #19146, #6309 ) ;
#19512 = CARTESIAN_POINT ( 'NONE',  ( -0.0001924259990621056968, 0.4692913385826771866, 0.1992150590373740204 ) ) ;
#19513 = DIRECTION ( 'NONE',  ( -0.000000000000000000, 1.000000000000000000, -0.000000000000000000 ) ) ;
#19514 = B_SPLINE_CURVE_WITH_KNOTS ( 'NONE', 3,
 ( #15205, #8691, #6578, #19575, #23949, #4585 ),
 .UNSPECIFIED., .F., .F.,
 ( 4, 2, 4 ),
 ( 0.000000000000000000, 0.2500000000000000000, 0.5000000000000000000 ),
 .UNSPECIFIED. ) ;
#19515 = EDGE_CURVE ( 'NONE', #17328, #4894, #24561, .T. ) ;
#19516 = CARTESIAN_POINT ( 'NONE',  ( 0.5526079293737398146, 0.1480156394741914405, 0.9399606299212598381 ) ) ;
#19517 = CARTESIAN_POINT ( 'NONE',  ( 0.1610509776512037416, -0.4407912692718771175, 0.07637795275590551769 ) ) ;
#19518 = EDGE_LOOP ( 'NONE', ( #25448, #25402, #7878, #16857 ) ) ;
#19519 = PRODUCT_DEFINITION_SHAPE ( 'NONE', 'NONE',  #11889 ) ;
#19520 = FACE_OUTER_BOUND ( 'NONE', #14953, .T. ) ;
#19521 = EDGE_CURVE ( 'NONE', #2487, #22124, #14749, .T. ) ;
#19522 = CIRCLE ( 'NONE', #7330, 0.2395669291338582696 ) ;
#19523 = EDGE_CURVE ( 'NONE', #10266, #6015, #1220, .T. ) ;
#19524 = AXIS2_PLACEMENT_3D ( 'NONE', #7475, #7067, #9296 ) ;
#19525 = ADVANCED_FACE ( 'NONE', ( #8135, #16744, #14797, #1625, #25505 ), #16601, .T. ) ;
#19526 = ORIENTED_EDGE ( 'NONE', *, *, #11442, .T. ) ;
#19527 = EDGE_CURVE ( 'NONE', #20809, #2885, #25212, .T. ) ;
#19528 = ORIENTED_EDGE ( 'NONE', *, *, #18506, .F. ) ;
#19529 = B_SPLINE_CURVE_WITH_KNOTS ( 'NONE', 3,
 ( #17558, #2563, #10632, #24316, #4964, #2825 ),
 .UNSPECIFIED., .F., .F.,
 ( 4, 2, 4 ),
 ( 0.6902184472752670441, 0.6915327610580700446, 0.6928470748408740443 ),
 .UNSPECIFIED. ) ;
#19530 = CARTESIAN_POINT ( 'NONE',  ( 0.4301590433675085978, -0.3771696032822019484, 0.9399606299212598381 ) ) ;
#19531 = EDGE_CURVE ( 'NONE', #25409, #10563, #6171, .T. ) ;
#19532 = CARTESIAN_POINT ( 'NONE',  ( 0.4621283342336283129, 0.08168108835549410529, 0.07637549214372854611 ) ) ;
#19533 = DIRECTION ( 'NONE',  ( -0.9575713609010866323, -0.2881962678142118706, -3.529386369048878649E-17 ) ) ;
#19534 = ORIENTED_EDGE ( 'NONE', *, *, #25183, .F. ) ;
#19535 = CARTESIAN_POINT ( 'NONE',  ( -0.5511811023268710086, 0.000000000000000000, 1.747047244094488194 ) ) ;
#19536 = ORIENTED_EDGE ( 'NONE', *, *, #24552, .F. ) ;
#19537 = SURFACE_SIDE_STYLE ('',( #24187 ) ) ;
#19538 = LINE ( 'NONE', #26429, #9018 ) ;
#19539 = VERTEX_POINT ( 'NONE', #6017 ) ;
#19540 = AXIS2_PLACEMENT_3D ( 'NONE', #4245, #19210, #19065 ) ;
#19541 = CARTESIAN_POINT ( 'NONE',  ( -0.4626586504047134341, 0.000000000000000000, -0.2204724409448818867 ) ) ;
#19542 = AXIS2_PLACEMENT_3D ( 'NONE', #26894, #2865, #9505 ) ;
#19543 = CARTESIAN_POINT ( 'NONE',  ( -0.4771018889076559244, 0.3804760601893846794, 0.2362204724409449064 ) ) ;
#19544 = ORIENTED_EDGE ( 'NONE', *, *, #7789, .F. ) ;
#19545 = DIRECTION ( 'NONE',  ( 0.000000000000000000, 1.000000000000000000, 0.000000000000000000 ) ) ;
#19546 = CARTESIAN_POINT ( 'NONE',  ( -0.4669911931914798586, -0.1585706980422492696, -1.569881889763779625 ) ) ;
#19547 = CARTESIAN_POINT ( 'NONE',  ( 0.000000000000000000, 0.000000000000000000, -3.110236220451535694 ) ) ;
#19548 = CARTESIAN_POINT ( 'NONE',  ( 0.4555658499976260600, 0.06001958459474954211, -1.928289503579140529 ) ) ;
#19549 = ( REPRESENTATION_RELATIONSHIP ('NONE','NONE', #12434, #6338 ) REPRESENTATION_RELATIONSHIP_WITH_TRANSFORMATION ( #16099 )SHAPE_REPRESENTATION_RELATIONSHIP( ) ) ;
#19550 = APPLICATION_CONTEXT ( 'automotive_design' ) ;
#19551 = CARTESIAN_POINT ( 'NONE',  ( 0.4986013261500205074, 6.106105181202481056E-17, -0.1756889763779527769 ) ) ;
#19552 = ADVANCED_FACE ( 'NONE', ( #27345 ), #14358, .T. ) ;
#19553 = DIRECTION ( 'NONE',  ( 0.6427876096865396960, 0.7660444431189776804, -0.000000000000000000 ) ) ;
#19554 = CARTESIAN_POINT ( 'NONE',  ( -0.6305589872448129629, -0.09245759066824232875, 0.2329406148073893679 ) ) ;
#19555 = DIRECTION ( 'NONE',  ( 0.000000000000000000, 0.000000000000000000, -1.000000000000000000 ) ) ;
#19556 = CARTESIAN_POINT ( 'NONE',  ( 0.3242071728275346953, -0.4225965726692721969, 1.747047244094488194 ) ) ;
#19557 = EDGE_CURVE ( 'NONE', #27881, #14806, #16062, .T. ) ;
#19558 = ( NAMED_UNIT ( * ) PLANE_ANGLE_UNIT ( ) SI_UNIT ( $, .RADIAN. ) ) ;
#19559 = CIRCLE ( 'NONE', #27690, 0.01377952755905511965 ) ;
#19560 = VERTEX_POINT ( 'NONE', #23401 ) ;
#19561 = DIRECTION ( 'NONE',  ( -1.224646799147353207E-16, 1.000000000000000000, 0.000000000000000000 ) ) ;
#19562 = AXIS2_PLACEMENT_3D ( 'NONE', #13529, #17503, #24405 ) ;
#19563 = CARTESIAN_POINT ( 'NONE',  ( -0.4783464566929133688, -0.4724409448818898127, 0.8182917201112815953 ) ) ;
#19564 = CARTESIAN_POINT ( 'NONE',  ( 0.3543307086614173040, -1.934043700787401319E-18, 0.000000000000000000 ) ) ;
#19565 = ORIENTED_EDGE ( 'NONE', *, *, #22601, .F. ) ;
#19566 = DIRECTION ( 'NONE',  ( -0.2036417511401759084, -0.4895227362422917006, -0.8478782506317888989 ) ) ;
#19567 = EDGE_CURVE ( 'NONE', #25542, #19740, #25985, .T. ) ;
#19568 = ORIENTED_EDGE ( 'NONE', *, *, #11269, .F. ) ;
#19569 = CARTESIAN_POINT ( 'NONE',  ( -0.6587140840999922142, 0.006880217451793542785, -0.07874015870966023789 ) ) ;
#19570 = ORIENTED_EDGE ( 'NONE', *, *, #25984, .T. ) ;
#19571 = CIRCLE ( 'NONE', #7375, 0.3771653543307086909 ) ;
#19572 = CARTESIAN_POINT ( 'NONE',  ( 2.632951206231566310, -0.4724409448818898127, 0.8182917201112794858 ) ) ;
#19573 = EDGE_CURVE ( 'NONE', #26656, #18025, #20875, .T. ) ;
#19574 = CARTESIAN_POINT ( 'NONE',  ( 0.5188388941967637669, -0.1188778293835250077, 0.1322818204150990051 ) ) ;
#19575 = CARTESIAN_POINT ( 'NONE',  ( -0.4015002836661830110, -0.2311469024283132612, 0.1494804571819171590 ) ) ;
#19576 = CIRCLE ( 'NONE', #11876, 0.4606299212598425341 ) ;
#19577 = DIRECTION ( 'NONE',  ( -0.000000000000000000, -1.000000000000000000, -0.000000000000000000 ) ) ;
#19578 = TOROIDAL_SURFACE ( 'NONE', #19511, 0.4232283464566928832, 0.07677165354330708902 ) ;
#19579 = CARTESIAN_POINT ( 'NONE',  ( -0.02917857698710797643, -0.4446035140077002623, -1.934055118110236338 ) ) ;
#19580 = CARTESIAN_POINT ( 'NONE',  ( -0.2962590301041579388, -0.2272836761397900585, -3.115157480314960647 ) ) ;
#19581 = DIRECTION ( 'NONE',  ( 0.000000000000000000, 1.000000000000000000, 0.000000000000000000 ) ) ;
#19582 = CARTESIAN_POINT ( 'NONE',  ( 0.2965233727166234345, 0.3524965443697388179, 0.1639447408612718093 ) ) ;
#19583 = CARTESIAN_POINT ( 'NONE',  ( 0.06894484415506239861, -0.05111597790242464190, -0.4724409448818898127 ) ) ;
#19584 = VECTOR ( 'NONE', #23070, 39.37007874015748143 ) ;
#19585 = ORIENTED_EDGE ( 'NONE', *, *, #7479, .F. ) ;
#19586 = CARTESIAN_POINT ( 'NONE',  ( 0.1516263115863346334, -0.1971492568089271424, 0.4530651079966787620 ) ) ;
#19588 = EDGE_CURVE ( 'NONE', #16922, #24495, #3701, .T. ) ;
#19587 = CIRCLE ( 'NONE', #12360, 0.2952755905511805223 ) ;
#19589 = VERTEX_POINT ( 'NONE', #10377 ) ;
#19590 = AXIS2_PLACEMENT_3D ( 'NONE', #24568, #4945, #20482 ) ;
#19591 = ORIENTED_EDGE ( 'NONE', *, *, #6447, .T. ) ;
#19592 = DIRECTION ( 'NONE',  ( 0.8660254037844382635, -0.5000000000000005551, 0.000000000000000000 ) ) ;
#19593 = CARTESIAN_POINT ( 'NONE',  ( 0.3680051700917442714, 0.4526932812344531265, 0.000000000000000000 ) ) ;
#19594 = CARTESIAN_POINT ( 'NONE',  ( 0.03349795313264332386, 0.5118110236220472231, 1.766732283464566899 ) ) ;
#19595 = EDGE_CURVE ( 'NONE', #19464, #21723, #20101, .T. ) ;
#19596 = VERTEX_POINT ( 'NONE', #4037 ) ;
#19597 = ( LENGTH_UNIT ( ) NAMED_UNIT ( * ) SI_UNIT ( $, .METRE. ) ) ;
#19598 = ORIENTED_EDGE ( 'NONE', *, *, #4679, .T. ) ;
#19599 = VERTEX_POINT ( 'NONE', #16463 ) ;
#19601 = CARTESIAN_POINT ( 'NONE',  ( 0.3551931031211721379, 0.04679574315772513232, -3.115157480314960647 ) ) ;
#19600 = DIRECTION ( 'NONE',  ( 1.000000000000000000, 0.000000000000000000, -0.000000000000000000 ) ) ;
#19602 = ORIENTED_EDGE ( 'NONE', *, *, #26134, .T. ) ;
#19603 = EDGE_LOOP ( 'NONE', ( #1907, #977, #25288, #3398 ) ) ;
#19604 = DIRECTION ( 'NONE',  ( 0.000000000000000000, 0.000000000000000000, 1.000000000000000000 ) ) ;
#19605 = ( NAMED_UNIT ( * ) SI_UNIT ( $, .STERADIAN. ) SOLID_ANGLE_UNIT ( ) ) ;
#19606 = CARTESIAN_POINT ( 'NONE',  ( -0.3223547283257516272, 0.3832433309296771617, 0.2574803149606298969 ) ) ;
#19607 = AXIS2_PLACEMENT_3D ( 'NONE', #3051, #7174, #22282 ) ;
#19608 = CARTESIAN_POINT ( 'NONE',  ( -0.2211428102655905170, 0.2521176338356723168, 1.953740157480315043 ) ) ;
#19609 = EDGE_LOOP ( 'NONE', ( #10411, #18672, #21247, #26102 ) ) ;
#19610 = ORIENTED_EDGE ( 'NONE', *, *, #21879, .F. ) ;
#19611 = ORIENTED_EDGE ( 'NONE', *, *, #18545, .T. ) ;
#19612 = DIRECTION ( 'NONE',  ( -1.000000000000000000, 0.000000000000000000, 0.000000000000000000 ) ) ;
#19613 = ORIENTED_EDGE ( 'NONE', *, *, #20639, .T. ) ;
#19614 = ORIENTED_EDGE ( 'NONE', *, *, #5546, .F. ) ;
#19615 = ORIENTED_EDGE ( 'NONE', *, *, #24344, .F. ) ;
#19616 = DIRECTION ( 'NONE',  ( 0.000000000000000000, 0.000000000000000000, 1.000000000000000000 ) ) ;
#19617 = ADVANCED_FACE ( 'NONE', ( #23540 ), #3594, .T. ) ;
#19618 = AXIS2_PLACEMENT_3D ( 'NONE', #18051, #15971, #3366 ) ;
#19619 = CARTESIAN_POINT ( 'NONE',  ( 0.4245040230929275626, 0.8362902341299607301, -0.5517326013040156907 ) ) ;
#19620 = AXIS2_PLACEMENT_3D ( 'NONE', #7961, #9924, #1874 ) ;
#19621 = FACE_OUTER_BOUND ( 'NONE', #15393, .T. ) ;
#19622 = ORIENTED_EDGE ( 'NONE', *, *, #21879, .T. ) ;
#19623 = CARTESIAN_POINT ( 'NONE',  ( 0.6963683772927192761, 0.7698450987802122336, -0.01895869795567349525 ) ) ;
#19624 = ORIENTED_EDGE ( 'NONE', *, *, #18240, .F. ) ;
#19625 = CARTESIAN_POINT ( 'NONE',  ( -0.5144793533647340489, 0.1379038425975085413, 1.747047244094487972 ) ) ;
#19626 = DIRECTION ( 'NONE',  ( 0.000000000000000000, 0.000000000000000000, 1.000000000000000000 ) ) ;
#19627 = CIRCLE ( 'NONE', #20520, 0.4010740433761567081 ) ;
#19628 = LINE ( 'NONE', #15659, #10079 ) ;
#19629 = ORIENTED_EDGE ( 'NONE', *, *, #1371, .T. ) ;
#19630 = CARTESIAN_POINT ( 'NONE',  ( -1.466875984251968630E-17, 0.000000000000000000, -0.4566929133858267376 ) ) ;
#19631 = CARTESIAN_POINT ( 'NONE',  ( 0.5905511811023621549, 0.000000000000000000, 0.000000000000000000 ) ) ;
#19632 = EDGE_CURVE ( 'NONE', #5702, #13442, #3384, .T. ) ;
#19633 = DIRECTION ( 'NONE',  ( 0.000000000000000000, 0.000000000000000000, 1.000000000000000000 ) ) ;
#19634 = CARTESIAN_POINT ( 'NONE',  ( 0.1525037638700916243, 0.2314035372547589564, 0.4381595109572584690 ) ) ;
#19635 = ORIENTED_EDGE ( 'NONE', *, *, #705, .F. ) ;
#19636 = CIRCLE ( 'NONE', #20974, 0.3464566929133857665 ) ;
#19637 = CARTESIAN_POINT ( 'NONE',  ( -0.2720459371704843088, 0.3242117229735834716, 0.1377952755905511861 ) ) ;
#19638 = VERTEX_POINT ( 'NONE', #16895 ) ;
#19639 = CARTESIAN_POINT ( 'NONE',  ( -0.4897507849286801829, 0.08575075074550207732, 0.1615162260910394110 ) ) ;
#19640 = DIRECTION ( 'NONE',  ( -0.000000000000000000, -1.000000000000000000, -0.000000000000000000 ) ) ;
#19641 = CARTESIAN_POINT ( 'NONE',  ( -0.3528204557975102018, 0.06272520244122334332, 0.09506557083631544947 ) ) ;
#19642 = DIRECTION ( 'NONE',  ( -1.000000000000000000, 0.000000000000000000, 0.000000000000000000 ) ) ;
#19643 = ORIENTED_EDGE ( 'NONE', *, *, #15498, .F. ) ;
#19644 = CARTESIAN_POINT ( 'NONE',  ( 0.3642352168757886366, 0.4152525734086595088, 0.9399606299212598381 ) ) ;
#19645 = VERTEX_POINT ( 'NONE', #21271 ) ;
#19646 = AXIS2_PLACEMENT_3D ( 'NONE', #18598, #27527, #1663 ) ;
#19647 = LINE ( 'NONE', #11153, #19837 ) ;
#19648 = VERTEX_POINT ( 'NONE', #19137 ) ;
#19649 = CARTESIAN_POINT ( 'NONE',  ( 0.000000000000000000, 0.000000000000000000, 1.953740157480315043 ) ) ;
#19650 = DIRECTION ( 'NONE',  ( -0.2036417511401762970, 0.9790454724845841783, -1.198984999999999849E-16 ) ) ;
#19651 = CARTESIAN_POINT ( 'NONE',  ( 0.07874015748031495954, 0.03414999754207796723, -0.4724409448818898127 ) ) ;
#19652 = ORIENTED_EDGE ( 'NONE', *, *, #12698, .F. ) ;
#19653 = CARTESIAN_POINT ( 'NONE',  ( 0.000000000000000000, 0.000000000000000000, 0.1992125984251968684 ) ) ;
#19654 = EDGE_CURVE ( 'NONE', #16979, #2747, #14493, .T. ) ;
#19655 = AXIS2_PLACEMENT_3D ( 'NONE', #24336, #13596, #4980 ) ;
#19656 = CARTESIAN_POINT ( 'NONE',  ( -0.5177165354330708347, -0.4724409448818898127, 0.8182917201112794858 ) ) ;
#19657 = CARTESIAN_POINT ( 'NONE',  ( -0.09842519685039366473, 0.1968503937007873850, -3.456364829396323390 ) ) ;
#19658 = CARTESIAN_POINT ( 'NONE',  ( 0.5572789388089177676, -0.3225230913470072402, 0.2359405056200655770 ) ) ;
#19659 = VECTOR ( 'NONE', #18505, 39.37007874015748854 ) ;
#19660 = DIRECTION ( 'NONE',  ( 0.000000000000000000, -1.000000000000000000, 0.000000000000000000 ) ) ;
#19661 = DIRECTION ( 'NONE',  ( -1.000000000000000000, 0.000000000000000000, 0.000000000000000000 ) ) ;
#19662 = CARTESIAN_POINT ( 'NONE',  ( 0.000000000000000000, 0.4724409448818898127, -0.7874015748031496509 ) ) ;
#19663 = CARTESIAN_POINT ( 'NONE',  ( -0.1839420097223304074, 0.5417097841048854612, 0.9399606299212598381 ) ) ;
#19664 = EDGE_CURVE ( 'NONE', #13442, #4356, #8837, .T. ) ;
#19665 = DIRECTION ( 'NONE',  ( 0.000000000000000000, 0.000000000000000000, -1.000000000000000000 ) ) ;
#19666 = ORIENTED_EDGE ( 'NONE', *, *, #10264, .F. ) ;
#19667 = CARTESIAN_POINT ( 'NONE',  ( -0.4716287720758560176, -0.1069935333117274234, 0.2715646632661209425 ) ) ;
#19668 = ORIENTED_EDGE ( 'NONE', *, *, #3641, .F. ) ;
#19669 = ORIENTED_EDGE ( 'NONE', *, *, #17363, .F. ) ;
#19670 = ORIENTED_EDGE ( 'NONE', *, *, #81, .T. ) ;
#19671 = DIRECTION ( 'NONE',  ( 0.000000000000000000, -1.000000000000000000, 0.000000000000000000 ) ) ;
#19672 = DIRECTION ( 'NONE',  ( 0.000000000000000000, 0.000000000000000000, 1.000000000000000000 ) ) ;
#19673 = CARTESIAN_POINT ( 'NONE',  ( 0.5379714048901780288, 6.588249590315613132E-17, -0.2342519685039370358 ) ) ;
#19674 = ORIENTED_EDGE ( 'NONE', *, *, #15636, .F. ) ;
#19675 = CARTESIAN_POINT ( 'NONE',  ( -0.3122781343789607367, 0.4068940122751343869, -1.550196850393701142 ) ) ;
#19676 = CARTESIAN_POINT ( 'NONE',  ( 3.387491338582676985E-16, -0.6299212598425196763, 0.000000000000000000 ) ) ;
#19677 = ORIENTED_EDGE ( 'NONE', *, *, #22246, .F. ) ;
#19678 = AXIS2_PLACEMENT_3D ( 'NONE', #20139, #3168, #24792 ) ;
#19679 = DIRECTION ( 'NONE',  ( 0.000000000000000000, 0.000000000000000000, 1.000000000000000000 ) ) ;
#19680 = EDGE_CURVE ( 'NONE', #21206, #20489, #8680, .T. ) ;
#19681 = DIRECTION ( 'NONE',  ( 0.000000000000000000, 0.000000000000000000, -1.000000000000000000 ) ) ;
#19682 = DIRECTION ( 'NONE',  ( -0.000000000000000000, 1.000000000000000000, -0.000000000000000000 ) ) ;
#19683 = EDGE_CURVE ( 'NONE', #23783, #23531, #7029, .T. ) ;
#19684 = CARTESIAN_POINT ( 'NONE',  ( -0.09842519685039370636, -0.1673228346456692994, 2.049113738730807629E-17 ) ) ;
#19685 = DIRECTION ( 'NONE',  ( 8.659560562354932858E-17, 0.7071067811865474617, -0.7071067811865474617 ) ) ;
#19686 = EDGE_CURVE ( 'NONE', #6596, #1165, #17832, .T. ) ;
#19687 = ORIENTED_EDGE ( 'NONE', *, *, #12692, .T. ) ;
#19688 = DIRECTION ( 'NONE',  ( 0.000000000000000000, 0.000000000000000000, 1.000000000000000000 ) ) ;
#19689 = DIRECTION ( 'NONE',  ( -0.1772802999855984940, 0.000000000000000000, 0.9841604011730080703 ) ) ;
#19690 = CARTESIAN_POINT ( 'NONE',  ( 0.4270824798167662806, 0.2466292688014931900, -1.550196850393700920 ) ) ;
#19691 = EDGE_CURVE ( 'NONE', #20886, #24509, #11677, .T. ) ;
#19692 = CARTESIAN_POINT ( 'NONE',  ( 0.3030032861725032167, 0.3454440660767328364, -1.928289503579165620 ) ) ;
#19693 = DIRECTION ( 'NONE',  ( -1.000000000000000000, 0.000000000000000000, 0.000000000000000000 ) ) ;
#19694 = EDGE_CURVE ( 'NONE', #6066, #14064, #5667, .T. ) ;
#19695 = AXIS2_PLACEMENT_3D ( 'NONE', #22904, #14588, #22614 ) ;
#19696 = AXIS2_PLACEMENT_3D ( 'NONE', #27740, #10060, #1451 ) ;
#19697 = DIRECTION ( 'NONE',  ( -0.9009688679024191460, 0.4338837391175580094, 0.000000000000000000 ) ) ;
#19698 = DIRECTION ( 'NONE',  ( -1.000000000000000000, -1.224646799147356165E-16, 0.000000000000000000 ) ) ;
#19699 = DIRECTION ( 'NONE',  ( 1.000000000000000000, 0.000000000000000000, 0.000000000000000000 ) ) ;
#19700 = FACE_OUTER_BOUND ( 'NONE', #20375, .T. ) ;
#19701 = CARTESIAN_POINT ( 'NONE',  ( 1.692913385826771533, 0.07874015748031495954, 3.109831496062992451E-16 ) ) ;
#19702 = EDGE_LOOP ( 'NONE', ( #22343, #14584 ) ) ;
#19703 = CARTESIAN_POINT ( 'NONE',  ( -0.6633461167951516524, 0.01644978644481641730, -0.2363335391394980334 ) ) ;
#19704 = ORIENTED_EDGE ( 'NONE', *, *, #15552, .F. ) ;
#19705 = AXIS2_PLACEMENT_3D ( 'NONE', #12429, #27553, #17085 ) ;
#19706 = CARTESIAN_POINT ( 'NONE',  ( 0.1520645003235147619, 0.1970746732862649619, -0.4530975571996346818 ) ) ;
#19707 = CARTESIAN_POINT ( 'NONE',  ( 0.5187889641967551313, -0.1190953285357214675, 0.1322834645669291320 ) ) ;
#19708 = DIRECTION ( 'NONE',  ( -1.000000000000000000, 0.000000000000000000, 0.000000000000000000 ) ) ;
#19709 = CIRCLE ( 'NONE', #12923, 0.1181102362204718703 ) ;
#19710 = B_SPLINE_CURVE_WITH_KNOTS ( 'NONE', 3,
 ( #18238, #15605, #5413, #902, #2714, #11348 ),
 .UNSPECIFIED., .F., .F.,
 ( 4, 2, 4 ),
 ( 0.3864984308775630262, 0.3881911340211369743, 0.3898838371647120327 ),
 .UNSPECIFIED. ) ;
#19711 = CARTESIAN_POINT ( 'NONE',  ( 0.6397637795275591399, 9.160743773149492203E-17, 0.7480314960629921295 ) ) ;
#19712 = ADVANCED_FACE ( 'NONE', ( #24209 ), #10940, .T. ) ;
#19713 = AXIS2_PLACEMENT_3D ( 'NONE', #23598, #21874, #13948 ) ;
#19714 = CARTESIAN_POINT ( 'NONE',  ( -0.1431838228103958222, -0.4219236230597716575, -1.934055118110236560 ) ) ;
#19715 = CARTESIAN_POINT ( 'NONE',  ( -0.1651192144506347381, 0.3349073414798414139, -3.115157480314960647 ) ) ;
#19716 = DIRECTION ( 'NONE',  ( 0.7660444431189780135, 0.6427876096865392519, 0.000000000000000000 ) ) ;
#19717 = DIRECTION ( 'NONE',  ( -1.000000000000000000, 0.000000000000000000, 0.000000000000000000 ) ) ;
#19718 = LINE ( 'NONE', #15214, #9893 ) ;
#19719 = ADVANCED_FACE ( 'NONE', ( #10658, #4711 ), #26324, .T. ) ;
#19720 = ORIENTED_EDGE ( 'NONE', *, *, #26796, .T. ) ;
#19721 = DIRECTION ( 'NONE',  ( 0.000000000000000000, -1.000000000000000000, 0.000000000000000000 ) ) ;
#19722 = VERTEX_POINT ( 'NONE', #12916 ) ;
#19723 = CIRCLE ( 'NONE', #1676, 0.1771653543307086520 ) ;
#19724 = CARTESIAN_POINT ( 'NONE',  ( -0.1294857240059045234, -0.3542416573274181357, 0.1992125984251968684 ) ) ;
#19725 = DIRECTION ( 'NONE',  ( -1.000000000000000000, 0.000000000000000000, 0.000000000000000000 ) ) ;
#19726 = CARTESIAN_POINT ( 'NONE',  ( 0.1649135259617122706, 0.4856708409200614640, 1.766732283464566899 ) ) ;
#19727 = FACE_OUTER_BOUND ( 'NONE', #5629, .T. ) ;
#19728 = EDGE_CURVE ( 'NONE', #27804, #13542, #23307, .T. ) ;
#19729 = VERTEX_POINT ( 'NONE', #24072 ) ;
#19730 = EDGE_LOOP ( 'NONE', ( #20706, #9726, #7430, #5789 ) ) ;
#19732 = CARTESIAN_POINT ( 'NONE',  ( 0.2807137536170459802, 0.2462256503456008716, -3.115157480314960647 ) ) ;
#19731 = CARTESIAN_POINT ( 'NONE',  ( -0.6117062799105531523, 0.1085321106658068829, 0.2574803149606298969 ) ) ;
#19733 = ORIENTED_EDGE ( 'NONE', *, *, #16910, .T. ) ;
#19734 = CARTESIAN_POINT ( 'NONE',  ( 0.2249706821157846648, -0.6026734741281122298, -0.4922986699466661009 ) ) ;
#19735 = CARTESIAN_POINT ( 'NONE',  ( 0.5099673189336091372, -0.1157175986333315310, 0.1392975274251336271 ) ) ;
#19736 = CARTESIAN_POINT ( 'NONE',  ( -0.3175540113612215221, -0.1078280746903921422, 1.953740157480315043 ) ) ;
#19737 = ORIENTED_EDGE ( 'NONE', *, *, #27111, .T. ) ;
#19738 = ORIENTED_EDGE ( 'NONE', *, *, #10013, .T. ) ;
#19739 = CARTESIAN_POINT ( 'NONE',  ( -0.3937007874015748254, -1.131889763779527547, 1.386165176200252194E-16 ) ) ;
#19740 = VERTEX_POINT ( 'NONE', #246 ) ;
#19741 = ORIENTED_EDGE ( 'NONE', *, *, #272, .T. ) ;
#19742 = VERTEX_POINT ( 'NONE', #13187 ) ;
#19743 = CARTESIAN_POINT ( 'NONE',  ( -0.3606190329934327310, 0.4297690281277732338, 0.07676968503937006694 ) ) ;
#19744 = AXIS2_PLACEMENT_3D ( 'NONE', #13576, #2823, #11464 ) ;
#19745 = EDGE_CURVE ( 'NONE', #15470, #3752, #25065, .T. ) ;
#19746 = EDGE_CURVE ( 'NONE', #4474, #22287, #13352, .T. ) ;
#19747 = AXIS2_PLACEMENT_3D ( 'NONE', #15384, #9922, #18526 ) ;
#19748 = LINE ( 'NONE', #6348, #52 ) ;
#19749 = COLOUR_RGB ( '', 0.66274510, 0.83137255, 0.94901961) ;
#19750 = CARTESIAN_POINT ( 'NONE',  ( 0.6209510983512002147, 0.8905375929024810233, -0.1208886179116861054 ) ) ;
#19751 = EDGE_LOOP ( 'NONE', ( #8179, #16231, #2721 ) ) ;
#19752 = ADVANCED_FACE ( 'NONE', ( #23676 ), #11532, .T. ) ;
#19753 = CARTESIAN_POINT ( 'NONE',  ( 0.1522836969735573143, -0.1970374587079582740, -0.4531137400369409374 ) ) ;
#19754 = CARTESIAN_POINT ( 'NONE',  ( -0.5190368482393039606, -0.1180105360553399679, 0.3401591244667909186 ) ) ;
#19755 = CARTESIAN_POINT ( 'NONE',  ( -0.04957542349328453862, -0.06229891813554931657, -0.4653527282821430799 ) ) ;
#19756 = DIRECTION ( 'NONE',  ( 0.000000000000000000, 0.000000000000000000, -1.000000000000000000 ) ) ;
#19757 = CARTESIAN_POINT ( 'NONE',  ( 0.0006345105826660207057, 0.4803145415259078566, 0.2194422276352448742 ) ) ;
#19758 = AXIS2_PLACEMENT_3D ( 'NONE', #1678, #3644, #16945 ) ;
#19759 = CIRCLE ( 'NONE', #16220, 0.3135473077061334268 ) ;
#19760 = CARTESIAN_POINT ( 'NONE',  ( 0.4211031283173693462, -0.2438048970101359125, 0.09284957166162138842 ) ) ;
#19761 = ORIENTED_EDGE ( 'NONE', *, *, #18711, .T. ) ;
#19762 = CIRCLE ( 'NONE', #22462, 0.1181102362204718703 ) ;
#19763 = CARTESIAN_POINT ( 'NONE',  ( -0.3122922550262028363, 0.3730863453119290241, 0.2467937632973297712 ) ) ;
#19764 = CARTESIAN_POINT ( 'NONE',  ( 0.3075317527319106903, -0.1775220790475473265, 1.953740157480315043 ) ) ;
#19765 = VERTEX_POINT ( 'NONE', #19832 ) ;
#19766 = CARTESIAN_POINT ( 'NONE',  ( -0.02559055118110236185, 0.000000000000000000, 0.000000000000000000 ) ) ;
#19767 = DIRECTION ( 'NONE',  ( 0.000000000000000000, -1.000000000000000000, 0.000000000000000000 ) ) ;
#19768 = DIRECTION ( 'NONE',  ( 0.000000000000000000, 1.000000000000000000, 0.000000000000000000 ) ) ;
#19769 = CYLINDRICAL_SURFACE ( 'NONE', #7618, 0.1771653543307086798 ) ;
#19770 = AXIS2_PLACEMENT_3D ( 'NONE', #2819, #20209, #729 ) ;
#19771 = ORIENTED_EDGE ( 'NONE', *, *, #17592, .F. ) ;
#19772 = CARTESIAN_POINT ( 'NONE',  ( -0.2762247810519161129, -0.4783323773986413729, 0.9202755905511811330 ) ) ;
#19773 = CARTESIAN_POINT ( 'NONE',  ( 0.000000000000000000, 0.000000000000000000, 0.000000000000000000 ) ) ;
#19774 = VERTEX_POINT ( 'NONE', #11081 ) ;
#19775 = FACE_OUTER_BOUND ( 'NONE', #26493, .T. ) ;
#19776 = FACE_OUTER_BOUND ( 'NONE', #4123, .T. ) ;
#19777 = CARTESIAN_POINT ( 'NONE',  ( 0.2956505864974371400, 0.3532288989643546651, 0.1771653543307085410 ) ) ;
#19778 = DIRECTION ( 'NONE',  ( -0.2384530002628495460, 0.000000000000000000, -0.9711540385879292581 ) ) ;
#19779 = CARTESIAN_POINT ( 'NONE',  ( 0.3048711895202321220, -0.6348424542973617468, 0.1443310008636820574 ) ) ;
#19780 = ADVANCED_FACE ( 'NONE', ( #492, #19700 ), #20531, .T. ) ;
#19781 = CIRCLE ( 'NONE', #26533, 1.092519685039370136 ) ;
#19782 = EDGE_CURVE ( 'NONE', #3374, #11989, #25567, .T. ) ;
#19783 = AXIS2_PLACEMENT_3D ( 'NONE', #25735, #201, #17120 ) ;
#19784 = CARTESIAN_POINT ( 'NONE',  ( 0.03532354024591842501, -0.6299212598425196763, 0.000000000000000000 ) ) ;
#19785 = CARTESIAN_POINT ( 'NONE',  ( 0.5484420430263082791, -0.3174147232942853836, 0.1061598535660860931 ) ) ;
#19786 = AXIS2_PLACEMENT_3D ( 'NONE', #19114, #1605, #10209 ) ;
#19787 = CARTESIAN_POINT ( 'NONE',  ( -0.4858607088160732390, -0.2805118110236220486, 0.1771653543307086520 ) ) ;
#19788 = ORIENTED_EDGE ( 'NONE', *, *, #14443, .T. ) ;
#19789 = DIRECTION ( 'NONE',  ( 0.000000000000000000, 0.000000000000000000, 1.000000000000000000 ) ) ;
#19790 = CARTESIAN_POINT ( 'NONE',  ( 0.3772436174784425389, -0.4300830224589218265, 0.9399606299212598381 ) ) ;
#19791 = B_SPLINE_CURVE_WITH_KNOTS ( 'NONE', 3,
 ( #25387, #6, #23701, #6597, #27522, #18875 ),
 .UNSPECIFIED., .F., .F.,
 ( 4, 2, 4 ),
 ( 0.000000000000000000, 0.2500000000000000000, 0.5000000000000000000 ),
 .UNSPECIFIED. ) ;
#19792 = DIRECTION ( 'NONE',  ( 1.000000000000000000, 0.000000000000000000, 0.000000000000000000 ) ) ;
#19793 = DIRECTION ( 'NONE',  ( -1.000000000000000000, 0.000000000000000000, 0.000000000000000000 ) ) ;
#19794 = ORIENTED_EDGE ( 'NONE', *, *, #21026, .T. ) ;
#19795 = CIRCLE ( 'NONE', #7626, 0.3937007874015748254 ) ;
#19796 = ORIENTED_EDGE ( 'NONE', *, *, #17665, .F. ) ;
#19797 = EDGE_CURVE ( 'NONE', #26549, #17148, #5703, .T. ) ;
#19798 = AXIS2_PLACEMENT_3D ( 'NONE', #6422, #6837, #4301 ) ;
#19799 = DIRECTION ( 'NONE',  ( 0.000000000000000000, 0.9847781868929990079, -0.1738157720684100072 ) ) ;
#19800 = CARTESIAN_POINT ( 'NONE',  ( -0.7874015748031496509, 0.000000000000000000, -1.052618110236220428 ) ) ;
#19801 = CARTESIAN_POINT ( 'NONE',  ( 0.4681308612729627727, -0.1074986424507606286, 0.2362204724409450174 ) ) ;
#19802 = DIRECTION ( 'NONE',  ( 1.000000000000000000, 0.000000000000000000, 0.000000000000000000 ) ) ;
#19803 = EDGE_LOOP ( 'NONE', ( #21372, #25122, #21927, #4211 ) ) ;
#19804 = DIRECTION ( 'NONE',  ( 1.000000000000000000, 0.000000000000000000, 0.000000000000000000 ) ) ;
#19805 = CARTESIAN_POINT ( 'NONE',  ( -0.2990496115119744003, -0.6198172806990825956, 0.1322818203437346463 ) ) ;
#19806 = ADVANCED_FACE ( 'NONE', ( #19968, #15739 ), #2850, .T. ) ;
#19807 = DIRECTION ( 'NONE',  ( 0.000000000000000000, -1.000000000000000000, 0.000000000000000000 ) ) ;
#19808 = DIRECTION ( 'NONE',  ( 0.000000000000000000, 0.000000000000000000, -1.000000000000000000 ) ) ;
#19809 = CARTESIAN_POINT ( 'NONE',  ( -0.2720459371704843088, 0.3242117229735834716, 0.06102165354330708891 ) ) ;
#19810 = DIRECTION ( 'NONE',  ( 0.7071067818211370648, 0.7071067805519580807, -8.659560554583453627E-17 ) ) ;
#19811 = CARTESIAN_POINT ( 'NONE',  ( 6.750021728016536817E-17, 0.03937007874015751446, -0.5511811023975373702 ) ) ;
#19812 = VERTEX_POINT ( 'NONE', #5268 ) ;
#19813 = DIRECTION ( 'NONE',  ( 0.000000000000000000, 0.000000000000000000, -1.000000000000000000 ) ) ;
#19814 = CARTESIAN_POINT ( 'NONE',  ( -0.2362204724409449064, -0.4724409448818898127, 0.8182917201112794858 ) ) ;
#19815 = CARTESIAN_POINT ( 'NONE',  ( -0.4441657790094368230, 0.2564944395535841970, -1.550196850393700920 ) ) ;
#19816 = AXIS2_PLACEMENT_3D ( 'NONE', #20319, #14263, #9562 ) ;
#19817 = FACE_OUTER_BOUND ( 'NONE', #18558, .T. ) ;
#19818 = VECTOR ( 'NONE', #616, 39.37007874015748143 ) ;
#19819 = DIRECTION ( 'NONE',  ( 0.000000000000000000, 0.000000000000000000, -1.000000000000000000 ) ) ;
#19820 = AXIS2_PLACEMENT_3D ( 'NONE', #13441, #6798, #17253 ) ;
#19821 = DIRECTION ( 'NONE',  ( 0.000000000000000000, -1.000000000000000000, 0.000000000000000000 ) ) ;
#19822 = CARTESIAN_POINT ( 'NONE',  ( -0.1188866373884876204, 0.4438564651657459503, -1.928289503579154740 ) ) ;
#19823 = DIRECTION ( 'NONE',  ( -0.000000000000000000, 1.000000000000000000, -0.000000000000000000 ) ) ;
#19824 = CARTESIAN_POINT ( 'NONE',  ( -0.6305589872448129629, -0.05856602962723583133, -0.2382980545837602715 ) ) ;
#19825 = CARTESIAN_POINT ( 'NONE',  ( 0.000000000000000000, 0.000000000000000000, 0.7844728274238290666 ) ) ;
#19826 = EDGE_CURVE ( 'NONE', #11359, #9393, #23327, .T. ) ;
#19827 = SURFACE_SIDE_STYLE ('',( #10799 ) ) ;
#19828 = EDGE_CURVE ( 'NONE', #6574, #13188, #14184, .T. ) ;
#19829 = DIRECTION ( 'NONE',  ( 0.000000000000000000, 1.000000000000000000, 0.000000000000000000 ) ) ;
#19830 = CARTESIAN_POINT ( 'NONE',  ( -0.6010692214156458935, -0.5770957586667881944, 0.9615147744183358824 ) ) ;
#19831 = PRODUCT_RELATED_PRODUCT_CATEGORY ( 'part', '', ( #27402 ) ) ;
#19832 = CARTESIAN_POINT ( 'NONE',  ( 0.2019525613798653640, 0.3664466487725785426, 0.6347042139374529102 ) ) ;
#19833 = ORIENTED_EDGE ( 'NONE', *, *, #25383, .F. ) ;
#19834 = CYLINDRICAL_SURFACE ( 'NONE', #27203, 0.6212598425196850238 ) ;
#19835 = ADVANCED_FACE ( 'NONE', ( #16296 ), #13887, .T. ) ;
#19836 = DIRECTION ( 'NONE',  ( 1.000000000000000000, 0.000000000000000000, 0.000000000000000000 ) ) ;
#19837 = VECTOR ( 'NONE', #8895, 39.37007874015748143 ) ;
#19838 = CARTESIAN_POINT ( 'NONE',  ( -0.6562077975700097987, -8.659590551181102767E-14, 0.07874015748031495954 ) ) ;
#19839 = ORIENTED_EDGE ( 'NONE', *, *, #6447, .F. ) ;
#19840 = CARTESIAN_POINT ( 'NONE',  ( -0.4498374011142775575, 0.05926487674658489219, -1.934055118110236338 ) ) ;
#19841 = DIRECTION ( 'NONE',  ( 1.000000000000000000, 0.000000000000000000, 0.000000000000000000 ) ) ;
#19842 = AXIS2_PLACEMENT_3D ( 'NONE', #17457, #24224, #15364 ) ;
#19843 = CARTESIAN_POINT ( 'NONE',  ( 1.197070535079588716, 0.4724409448818898127, 1.197070535079588716 ) ) ;
#19844 = EDGE_CURVE ( 'NONE', #25987, #14125, #13605, .T. ) ;
#19845 = ADVANCED_FACE ( 'NONE', ( #5557, #625 ), #16013, .T. ) ;
#19846 = B_SPLINE_CURVE_WITH_KNOTS ( 'NONE', 3,
 ( #26985, #12285, #13993, #9885, #1551, #10025 ),
 .UNSPECIFIED., .F., .F.,
 ( 4, 2, 4 ),
 ( 0.9359046326922999537, 0.9375808709372039917, 0.9392571091821070306 ),
 .UNSPECIFIED. ) ;
#19847 = AXIS2_PLACEMENT_3D ( 'NONE', #16969, #1566, #25297 ) ;
#19848 = DIRECTION ( 'NONE',  ( 0.000000000000000000, 0.000000000000000000, -1.000000000000000000 ) ) ;
#19849 = PLANE ( 'NONE',  #10714 ) ;
#19850 = CARTESIAN_POINT ( 'NONE',  ( -0.5708661417322835607, 0.000000000000000000, 0.000000000000000000 ) ) ;
#19851 = DIRECTION ( 'NONE',  ( -1.000000000000000000, 0.000000000000000000, 0.000000000000000000 ) ) ;
#19852 = SHAPE_REPRESENTATION ( 'Barrel Cam', ( #11588 ), #18804 ) ;
#19853 = ORIENTED_EDGE ( 'NONE', *, *, #19986, .F. ) ;
#19854 = CARTESIAN_POINT ( 'NONE',  ( 0.2395669291338582696, 2.933848729453403498E-17, -0.4566929133858267376 ) ) ;
#19855 = AXIS2_PLACEMENT_3D ( 'NONE', #21383, #1883, #4147 ) ;
#19856 = CIRCLE ( 'NONE', #18488, 0.2256712916308122319 ) ;
#19857 = ORIENTED_EDGE ( 'NONE', *, *, #14605, .F. ) ;
#19858 = ORIENTED_EDGE ( 'NONE', *, *, #8794, .T. ) ;
#19859 = CARTESIAN_POINT ( 'NONE',  ( -0.4160174684701747894, 0.3320469875258716397, 0.1322810039474933141 ) ) ;
#19860 = CARTESIAN_POINT ( 'NONE',  ( -0.5118110236220473341, 0.06699590632655400002, 1.766732283464566899 ) ) ;
#19861 = CARTESIAN_POINT ( 'NONE',  ( 0.5118110236220472231, 0.03349795313260757468, 1.747047244094488194 ) ) ;
#19862 = FACE_OUTER_BOUND ( 'NONE', #27634, .T. ) ;
#19863 = ORIENTED_EDGE ( 'NONE', *, *, #13706, .T. ) ;
#19864 = ADVANCED_FACE ( 'NONE', ( #9214, #18245 ), #759, .T. ) ;
#19865 = CIRCLE ( 'NONE', #14486, 0.6881889763779527325 ) ;
#19866 = ORIENTED_EDGE ( 'NONE', *, *, #11853, .F. ) ;
#19867 = CARTESIAN_POINT ( 'NONE',  ( -0.3267488823401686893, 0.1886891683789005680, -3.100567304031762284 ) ) ;
#19868 = VERTEX_POINT ( 'NONE', #11620 ) ;
#19869 = CARTESIAN_POINT ( 'NONE',  ( -0.5385210225480960844, 0.4284847435812472183, 0.3401574803149606252 ) ) ;
#19870 = CARTESIAN_POINT ( 'NONE',  ( -0.3149606299212598381, 0.000000000000000000, -0.4448818897637791814 ) ) ;
#19871 = ADVANCED_FACE ( 'NONE', ( #24898, #3273 ), #26590, .T. ) ;
#19872 = ORIENTED_EDGE ( 'NONE', *, *, #13241, .F. ) ;
#19873 = CARTESIAN_POINT ( 'NONE',  ( 0.2041304421298423266, 0.2660793235464414264, 1.953740157480315043 ) ) ;
#19874 = VERTEX_POINT ( 'NONE', #24465 ) ;
#19875 = VERTEX_POINT ( 'NONE', #26880 ) ;
#19876 = VERTEX_POINT ( 'NONE', #5119 ) ;
#19877 = B_SPLINE_CURVE_WITH_KNOTS ( 'NONE', 3,
 ( #40, #25841, #6490, #8741 ),
 .UNSPECIFIED., .F., .F.,
 ( 4, 4 ),
 ( 0.9375808709372031036, 0.9392571091818440188 ),
 .UNSPECIFIED. ) ;
#19878 = DIRECTION ( 'NONE',  ( -0.8660254037844383745, -0.5000000000000003331, 0.000000000000000000 ) ) ;
#19879 = ADVANCED_FACE ( 'NONE', ( #13743 ), #7532, .F. ) ;
#19880 = ORIENTED_EDGE ( 'NONE', *, *, #4448, .F. ) ;
#19881 = ORIENTED_EDGE ( 'NONE', *, *, #26486, .T. ) ;
#19882 = DIRECTION ( 'NONE',  ( 0.000000000000000000, 1.224646799147353700E-16, 1.000000000000000000 ) ) ;
#19883 = CONICAL_SURFACE ( 'NONE', #73, 0.2012500529900838608, 1.047197550000000144 ) ;
#19884 = CONTEXT_DEPENDENT_SHAPE_REPRESENTATION ( #12860, #17700 ) ;
#19885 = CARTESIAN_POINT ( 'NONE',  ( 0.4898768902087983768, -2.712048031496063190E-16, -0.2362204724409449064 ) ) ;
#19886 = FACE_OUTER_BOUND ( 'NONE', #4073, .T. ) ;
#19887 = CARTESIAN_POINT ( 'NONE',  ( 0.000000000000000000, 0.000000000000000000, -0.01377952755905511792 ) ) ;
#19888 = ORIENTED_EDGE ( 'NONE', *, *, #17110, .F. ) ;
#19889 = ADVANCED_FACE ( 'NONE', ( #7387 ), #15185, .T. ) ;
#19890 = CONICAL_SURFACE ( 'NONE', #18513, 0.08582677165393072516, 0.7853981625000011624 ) ;
#19891 = DIRECTION ( 'NONE',  ( -1.000000000000000000, 1.224646799147353454E-16, 0.000000000000000000 ) ) ;
#19892 = CARTESIAN_POINT ( 'NONE',  ( 0.2669480828848183052, -0.2341512108694381034, 1.953740157480315043 ) ) ;
#19893 = CARTESIAN_POINT ( 'NONE',  ( -0.2122766679520244337, -0.5838685267775873822, 0.09684793308443542803 ) ) ;
#19894 = CARTESIAN_POINT ( 'NONE',  ( 0.000000000000000000, 0.000000000000000000, 0.2574803149606298969 ) ) ;
#19895 = CARTESIAN_POINT ( 'NONE',  ( 0.07874015748031495954, 0.02306930775746975082, -0.4684758132890252669 ) ) ;
#19896 = DIRECTION ( 'NONE',  ( -1.000000000000000000, 0.000000000000000000, 0.000000000000000000 ) ) ;
#19897 = CIRCLE ( 'NONE', #9491, 0.7874015748031496509 ) ;
#19898 = DIRECTION ( 'NONE',  ( 0.000000000000000000, 1.000000000000000000, 0.000000000000000000 ) ) ;
#19899 = ORIENTED_EDGE ( 'NONE', *, *, #2070, .T. ) ;
#19900 = CARTESIAN_POINT ( 'NONE',  ( 0.4084310843282699111, 0.3265597623324891785, 0.1392975274205298652 ) ) ;
#19901 = SHAPE_REPRESENTATION_RELATIONSHIP ( 'NONE' , 'NONE' ,  #1615, #8670 ) ;
#19902 = EDGE_CURVE ( 'NONE', #4205, #3117, #8402, .T. ) ;
#19903 = CARTESIAN_POINT ( 'NONE',  ( -0.4061284506584276199, -0.2351468520616558922, 0.07637795275590551769 ) ) ;
#19904 = ORIENTED_EDGE ( 'NONE', *, *, #22815, .F. ) ;
#19905 = ORIENTED_EDGE ( 'NONE', *, *, #8131, .F. ) ;
#19906 = CIRCLE ( 'NONE', #27135, 0.6212598425196850238 ) ;
#19907 = CARTESIAN_POINT ( 'NONE',  ( 0.000000000000000000, 0.000000000000000000, 0.01181102362204724393 ) ) ;
#19908 = CARTESIAN_POINT ( 'NONE',  ( -0.3411065095061436847, 0.06065137456822528028, 0.1276989850548526373 ) ) ;
#19909 = EDGE_LOOP ( 'NONE', ( #27174, #24838, #21477, #1739 ) ) ;
#19910 = CARTESIAN_POINT ( 'NONE',  ( 0.2442565704126269388, 0.4954197419817067960, 0.9399606299212598381 ) ) ;
#19911 = CARTESIAN_POINT ( 'NONE',  ( 0.000000000000000000, 0.5322834645669292097, -1.092739370078740131E-17 ) ) ;
#19912 = VERTEX_POINT ( 'NONE', #4002 ) ;
#19913 = CARTESIAN_POINT ( 'NONE',  ( 0.7874015748031496509, 0.000000000000000000, -1.052618110236220428 ) ) ;
#19914 = EDGE_CURVE ( 'NONE', #14586, #13676, #7504, .T. ) ;
#19915 = CARTESIAN_POINT ( 'NONE',  ( 0.000000000000000000, 0.000000000000000000, 0.07637795275590551769 ) ) ;
#19916 = DIRECTION ( 'NONE',  ( 0.000000000000000000, -1.000000000000000000, 0.000000000000000000 ) ) ;
#19917 = CARTESIAN_POINT ( 'NONE',  ( 0.000000000000000000, 0.000000000000000000, -0.05856299212598425896 ) ) ;
#19918 = CARTESIAN_POINT ( 'NONE',  ( 0.1259842519685039353, -1.446320346059429855E-17, -0.1181010187644645354 ) ) ;
#19919 = EDGE_CURVE ( 'NONE', #2920, #730, #25088, .T. ) ;
#19920 = AXIS2_PLACEMENT_3D ( 'NONE', #15557, #4789, #13408 ) ;
#19921 = CARTESIAN_POINT ( 'NONE',  ( 0.7874015748031496509, 5.862181872598426086E-06, -1.869015748010449007 ) ) ;
#19922 = DIRECTION ( 'NONE',  ( 0.000000000000000000, -0.000000000000000000, -1.000000000000000000 ) ) ;
#19923 = CARTESIAN_POINT ( 'NONE',  ( 0.4130706566799093316, 0.3346769814300175061, -0.5796775359605764733 ) ) ;
#19924 = PRESENTATION_LAYER_ASSIGNMENT (  '', '', ( #14057 ) ) ;
#19925 = DIRECTION ( 'NONE',  ( 0.7071067811865470176, 0.7071067811865480168, 0.000000000000000000 ) ) ;
#19926 = CARTESIAN_POINT ( 'NONE',  ( -0.5526079293736928522, -0.1480156394741928838, 0.9399606299212598381 ) ) ;
#19927 = CARTESIAN_POINT ( 'NONE',  ( 0.5905511811200284678, 0.07874015746264864668, 0.000000000000000000 ) ) ;
#19928 = DIRECTION ( 'NONE',  ( 0.000000000000000000, 0.000000000000000000, 1.000000000000000000 ) ) ;
#19929 = ORIENTED_EDGE ( 'NONE', *, *, #23570, .T. ) ;
#19930 = CARTESIAN_POINT ( 'NONE',  ( -0.4339912984563299436, -0.2498791196563492356, 0.2574803149606298969 ) ) ;
#19931 = B_SPLINE_CURVE_WITH_KNOTS ( 'NONE', 3,
 ( #3802, #14980, #6483, #19332, #19470, #2232 ),
 .UNSPECIFIED., .F., .F.,
 ( 4, 2, 4 ),
 ( 0.000000000000000000, 0.2500000000000000000, 0.5000000000000000000 ),
 .UNSPECIFIED. ) ;
#19932 = EDGE_CURVE ( 'NONE', #17699, #26673, #609, .T. ) ;
#19933 = VERTEX_POINT ( 'NONE', #8240 ) ;
#19934 = CIRCLE ( 'NONE', #122, 0.08582677165167480748 ) ;
#19935 = DIRECTION ( 'NONE',  ( 1.224646799147353207E-16, 1.000000000000000000, -0.000000000000000000 ) ) ;
#19936 = DIRECTION ( 'NONE',  ( 1.000000000000000000, 0.000000000000000000, 0.000000000000000000 ) ) ;
#19937 = VERTEX_POINT ( 'NONE', #18960 ) ;
#19938 = DIRECTION ( 'NONE',  ( 1.000000000000000000, 0.000000000000000000, 0.000000000000000000 ) ) ;
#19939 = ORIENTED_EDGE ( 'NONE', *, *, #20548, .T. ) ;
#19940 = CARTESIAN_POINT ( 'NONE',  ( -0.4068916527368352520, 0.3122765577853303109, -1.550196850393700920 ) ) ;
#19941 = DIRECTION ( 'NONE',  ( 0.000000000000000000, 0.000000000000000000, 1.000000000000000000 ) ) ;
#19942 = ORIENTED_EDGE ( 'NONE', *, *, #17530, .F. ) ;
#19943 = CIRCLE ( 'NONE', #24441, 0.3771653543307086909 ) ;
#19944 = CARTESIAN_POINT ( 'NONE',  ( 0.7217751814634446594, -0.1639319465208047555, 0.2161412452816648122 ) ) ;
#19945 = CARTESIAN_POINT ( 'NONE',  ( 0.7873253891977465280, 0.3967224475386726956, 0.1736657078145811273 ) ) ;
#19946 = CYLINDRICAL_SURFACE ( 'NONE', #5839, 0.3771653543307086909 ) ;
#19947 = CARTESIAN_POINT ( 'NONE',  ( 0.000000000000000000, 0.000000000000000000, -0.006889763779527558960 ) ) ;
#19948 = ORIENTED_EDGE ( 'NONE', *, *, #19664, .F. ) ;
#19949 = CARTESIAN_POINT ( 'NONE',  ( 0.01298928997750990744, 0.3147564789080253278, -3.646005713789110203 ) ) ;
#19950 = DIRECTION ( 'NONE',  ( 0.000000000000000000, 0.000000000000000000, -1.000000000000000000 ) ) ;
#19951 = CARTESIAN_POINT ( 'NONE',  ( 0.1649135259639241124, 0.4856708409191630715, -1.550196850393700920 ) ) ;
#19952 = CIRCLE ( 'NONE', #18173, 0.1298643763538141760 ) ;
#19953 = ORIENTED_EDGE ( 'NONE', *, *, #6623, .F. ) ;
#19954 = CARTESIAN_POINT ( 'NONE',  ( 0.4438564651657541105, -0.1188866373884811950, -1.928289503579147857 ) ) ;
#19955 = CARTESIAN_POINT ( 'NONE',  ( 0.1775991818008376133, 0.5230301363771421297, 0.9202755905511811330 ) ) ;
#19956 = CARTESIAN_POINT ( 'NONE',  ( 0.0005056364805201059732, 0.3583524373864921952, 0.1805249803418951804 ) ) ;
#19957 = DIRECTION ( 'NONE',  ( 1.000000000000000000, 0.000000000000000000, 0.000000000000000000 ) ) ;
#19958 = CARTESIAN_POINT ( 'NONE',  ( -0.5905511811023621549, -0.4526313213353574949, 0.9943460912301771426 ) ) ;
#19959 = AXIS2_PLACEMENT_3D ( 'NONE', #22631, #3253, #5542 ) ;
#19960 = B_SPLINE_CURVE_WITH_KNOTS ( 'NONE', 3,
 ( #18167, #22577, #9276, #10271, #23012, #12257, #20879, #22868 ),
 .UNSPECIFIED., .F., .F.,
 ( 4, 2, 2, 4 ),
 ( 0.000000000000000000, 0.1250000000000001388, 0.2500000000000002776, 0.5000000000000000000 ),
 .UNSPECIFIED. ) ;
#19961 = EDGE_CURVE ( 'NONE', #13094, #21206, #16994, .T. ) ;
#19962 = DIRECTION ( 'NONE',  ( -0.8660254037844382635, 0.5000000000000005551, 0.000000000000000000 ) ) ;
#19963 = CARTESIAN_POINT ( 'NONE',  ( 0.2992781133269515892, -0.6197069291944330427, 0.3401574803149606252 ) ) ;
#19964 = CARTESIAN_POINT ( 'NONE',  ( -0.1771653543307086520, -5.663984251968503442E-18, 0.000000000000000000 ) ) ;
#19965 = CARTESIAN_POINT ( 'NONE',  ( 0.3937007873768824662, 0.000000000000000000, -0.1377952755696461029 ) ) ;
#19966 = ADVANCED_FACE ( 'NONE', ( #25325 ), #1873, .T. ) ;
#19967 = CARTESIAN_POINT ( 'NONE',  ( -0.0006812437162536292114, 0.6577569867595576270, 0.1461456498329627707 ) ) ;
#19968 = FACE_BOUND ( 'NONE', #26241, .T. ) ;
#19969 = DIRECTION ( 'NONE',  ( -1.000000000000000000, 0.000000000000000000, 0.000000000000000000 ) ) ;
#19970 = ORIENTED_EDGE ( 'NONE', *, *, #9485, .T. ) ;
#19971 = AXIS2_PLACEMENT_3D ( 'NONE', #21088, #12748, #1593 ) ;
#19972 = CARTESIAN_POINT ( 'NONE',  ( -0.7121770198535963825, 0.1553695409075332712, -0.09097790435992263169 ) ) ;
#19973 = ORIENTED_EDGE ( 'NONE', *, *, #26244, .F. ) ;
#19974 = AXIS2_PLACEMENT_3D ( 'NONE', #8115, #20819, #23093 ) ;
#19975 = CARTESIAN_POINT ( 'NONE',  ( -3.616083068348483797E-17, -0.2952755905511810774, 0.2637795275590551491 ) ) ;
#19976 = DIRECTION ( 'NONE',  ( -1.000000000000000000, 0.000000000000000000, 0.000000000000000000 ) ) ;
#19977 = ADVANCED_FACE ( 'NONE', ( #10482 ), #13369, .T. ) ;
#19978 = CARTESIAN_POINT ( 'NONE',  ( 0.3339160553493877859, 0.000000000000000000, -1.052618110236220428 ) ) ;
#19979 = AXIS2_PLACEMENT_3D ( 'NONE', #17532, #13558, #17790 ) ;
#19980 = CARTESIAN_POINT ( 'NONE',  ( -0.1970998888482735634, -0.3995939286812472124, -1.934055118110236338 ) ) ;
#19981 = CARTESIAN_POINT ( 'NONE',  ( 0.3765118517642104257, -0.02464264302293790732, -3.100567304031763172 ) ) ;
#19982 = DIRECTION ( 'NONE',  ( 0.000000000000000000, 0.000000000000000000, -1.000000000000000000 ) ) ;
#19983 = CARTESIAN_POINT ( 'NONE',  ( -0.1968503937007874127, 0.07874015748031495954, 0.04546065111729331171 ) ) ;
#19984 = CARTESIAN_POINT ( 'NONE',  ( 1.877524803149606209E-16, 0.000000000000000000, 0.000000000000000000 ) ) ;
#19985 = ORIENTED_EDGE ( 'NONE', *, *, #26961, .F. ) ;
#19986 = EDGE_CURVE ( 'NONE', #3579, #11103, #26428, .T. ) ;
#19987 = CARTESIAN_POINT ( 'NONE',  ( -0.4793172621399190425, -0.1288129352161815622, -1.569881889763780070 ) ) ;
#19988 = AXIS2_PLACEMENT_3D ( 'NONE', #15518, #11256, #19461 ) ;
#19989 = APPLICATION_PROTOCOL_DEFINITION ( 'draft international standard', 'automotive_design', 1998, #4937 ) ;
#19990 = CARTESIAN_POINT ( 'NONE',  ( -0.0004405150045524263542, 0.6212597256746514862, 0.2574819594177531479 ) ) ;
#19991 = CONICAL_SURFACE ( 'NONE', #18629, 0.08582677165393072516, 0.7853981625000011624 ) ;
#19992 = ORIENTED_EDGE ( 'NONE', *, *, #6732, .F. ) ;
#19993 = EDGE_CURVE ( 'NONE', #14972, #20570, #6616, .T. ) ;
#19994 = CARTESIAN_POINT ( 'NONE',  ( 0.4890020181333677995, -0.1109469068267140701, 0.3080453759527908009 ) ) ;
#19995 = CARTESIAN_POINT ( 'NONE',  ( -0.6233905297002754198, -0.4658379333990866900, 0.9954608945794582997 ) ) ;
#19996 = CARTESIAN_POINT ( 'NONE',  ( -0.4954415918530867824, -0.1327036767659759697, 1.747047244094488194 ) ) ;
#19997 = EDGE_LOOP ( 'NONE', ( #26991, #26131, #4374, #18322 ) ) ;
#19998 = ( NAMED_UNIT ( * ) PLANE_ANGLE_UNIT ( ) SI_UNIT ( $, .RADIAN. ) ) ;
#19999 = TOROIDAL_SURFACE ( 'NONE', #16877, 0.3740157480314960647, 0.03937007874015747977 ) ;
#20000 = CARTESIAN_POINT ( 'NONE',  ( 0.3702005978258584573, 0.04877294052296160531, -3.115157480314960647 ) ) ;
#20001 = CIRCLE ( 'NONE', #8284, 0.3543307086367249448 ) ;
#20002 = ORIENTED_EDGE ( 'NONE', *, *, #4119, .T. ) ;
#20003 = DIRECTION ( 'NONE',  ( 0.000000000000000000, 0.000000000000000000, -1.000000000000000000 ) ) ;
#20004 = CARTESIAN_POINT ( 'NONE',  ( 0.1490609433615242285, 0.2393035190771452825, -0.4144858534716441278 ) ) ;
#20005 = CARTESIAN_POINT ( 'NONE',  ( -0.3324885138898231451, -0.04380447413659061678, 1.953740157480315043 ) ) ;
#20006 = ORIENTED_EDGE ( 'NONE', *, *, #26211, .F. ) ;
#20007 = DIRECTION ( 'NONE',  ( 1.000000000000000000, 0.000000000000000000, 0.000000000000000000 ) ) ;
#20008 = ORIENTED_EDGE ( 'NONE', *, *, #22423, .F. ) ;
#20009 = EDGE_LOOP ( 'NONE', ( #1985, #23887, #19326, #11457 ) ) ;
#20010 = EDGE_LOOP ( 'NONE', ( #26031, #18172, #19502, #23090 ) ) ;
#20011 = CARTESIAN_POINT ( 'NONE',  ( -0.3214446924536846772, 0.3840069416942866742, 0.09685039370078740717 ) ) ;
#20012 = CIRCLE ( 'NONE', #8294, 0.1181102362204718703 ) ;
#20013 = SHAPE_REPRESENTATION ( 'Shaft Seal 20x35x7', ( #11588 ), #9813 ) ;
#20014 = EDGE_CURVE ( 'NONE', #11261, #12544, #26127, .T. ) ;
#20015 = DIRECTION ( 'NONE',  ( 1.000000000000000000, 0.000000000000000000, 0.000000000000000000 ) ) ;
#20016 = CARTESIAN_POINT ( 'NONE',  ( -0.02063739440585312876, 0.1968503937007874127, -3.195955311827340051 ) ) ;
#20017 = CARTESIAN_POINT ( 'NONE',  ( 0.7871730179869745880, 0.4038169352867496120, 0.1713250154738354125 ) ) ;
#20018 = EDGE_CURVE ( 'NONE', #16610, #11062, #18814, .T. ) ;
#20019 = CIRCLE ( 'NONE', #23638, 0.1082677165354330728 ) ;
#20020 = DIRECTION ( 'NONE',  ( 0.000000000000000000, -0.000000000000000000, -1.000000000000000000 ) ) ;
#20021 = EDGE_CURVE ( 'NONE', #18631, #18101, #3410, .T. ) ;
#20022 = CIRCLE ( 'NONE', #11450, 0.01181102362204724046 ) ;
#20023 = CARTESIAN_POINT ( 'NONE',  ( -0.1570220809524473238, 0.3184841198566425446, 1.953740157480315043 ) ) ;
#20024 = ADVANCED_FACE ( 'NONE', ( #23372, #18527 ), #14622, .T. ) ;
#20025 = CARTESIAN_POINT ( 'NONE',  ( 0.000000000000000000, 0.000000000000000000, 0.07637795275590551769 ) ) ;
#20026 = CARTESIAN_POINT ( 'NONE',  ( -0.5905511811023621549, -0.6995255587508188988, 0.000000000000000000 ) ) ;
#20027 = DIRECTION ( 'NONE',  ( 0.000000000000000000, 0.000000000000000000, -1.000000000000000000 ) ) ;
#20028 = EDGE_CURVE ( 'NONE', #20147, #26096, #14280, .T. ) ;
#20029 = CARTESIAN_POINT ( 'NONE',  ( 0.07874015748031495954, -0.02322203878497701435, -0.4680927705512025194 ) ) ;
#20030 = CARTESIAN_POINT ( 'NONE',  ( 0.0006479495459715539770, 0.5014297259271046636, 0.1643955689159069811 ) ) ;
#20031 = AXIS2_PLACEMENT_3D ( 'NONE', #3989, #26689, #19792 ) ;
#20032 = VERTEX_POINT ( 'NONE', #5706 ) ;
#20033 = CARTESIAN_POINT ( 'NONE',  ( -0.3149606299212598381, -0.5905511811023621549, 7.232166136696967594E-17 ) ) ;
#20034 = ORIENTED_EDGE ( 'NONE', *, *, #24999, .T. ) ;
#20035 = DIRECTION ( 'NONE',  ( 1.000000000000000000, 0.000000000000000000, 0.000000000000000000 ) ) ;
#20036 = CARTESIAN_POINT ( 'NONE',  ( 0.1141156591737397391, -0.3362580771779613009, 1.953740157480315043 ) ) ;
#20037 = ORIENTED_EDGE ( 'NONE', *, *, #2917, .F. ) ;
#20038 = DIRECTION ( 'NONE',  ( -0.000000000000000000, -0.000000000000000000, -1.000000000000000000 ) ) ;
#20039 = ORIENTED_EDGE ( 'NONE', *, *, #26820, .F. ) ;
#20040 = AXIS2_PLACEMENT_3D ( 'NONE', #27370, #16629, #23285 ) ;
#20041 = DIRECTION ( 'NONE',  ( 0.000000000000000000, 0.000000000000000000, -1.000000000000000000 ) ) ;
#20042 = CARTESIAN_POINT ( 'NONE',  ( 1.197070535079588716, 0.07874015748031495954, 1.197070535079588716 ) ) ;
#20043 = AXIS2_PLACEMENT_3D ( 'NONE', #24986, #5647, #17218 ) ;
#20044 = ORIENTED_EDGE ( 'NONE', *, *, #20733, .F. ) ;
#20045 = CARTESIAN_POINT ( 'NONE',  ( 0.2860899518037664513, 0.4954156765914491944, 0.9399606299212598381 ) ) ;
#20046 = ORIENTED_EDGE ( 'NONE', *, *, #26644, .F. ) ;
#20047 = DIRECTION ( 'NONE',  ( 1.000000000000000000, 0.000000000000000000, -0.000000000000000000 ) ) ;
#20048 = CARTESIAN_POINT ( 'NONE',  ( -0.5949363243629232079, -0.1357903337134990229, 0.1062972440944881941 ) ) ;
#20049 = CARTESIAN_POINT ( 'NONE',  ( 0.000000000000000000, 0.1136516277932332619, 0.1968503937007874127 ) ) ;
#20050 = DIRECTION ( 'NONE',  ( 0.000000000000000000, 0.000000000000000000, 1.000000000000000000 ) ) ;
#20051 = DIRECTION ( 'NONE',  ( 1.000000000000000000, 0.000000000000000000, 0.000000000000000000 ) ) ;
#20052 = DIRECTION ( 'NONE',  ( -0.2036417511401762970, -0.9790454724845841783, 0.000000000000000000 ) ) ;
#20053 = CIRCLE ( 'NONE', #20968, 0.6299212598425196763 ) ;
#20054 = EDGE_CURVE ( 'NONE', #27454, #27801, #14318, .T. ) ;
#20055 = DIRECTION ( 'NONE',  ( 0.000000000000000000, 0.000000000000000000, 1.000000000000000000 ) ) ;
#20056 = DIRECTION ( 'NONE',  ( -1.000000000000000000, 0.000000000000000000, 0.000000000000000000 ) ) ;
#20057 = DIRECTION ( 'NONE',  ( 0.000000000000000000, 1.000000000000000000, 0.000000000000000000 ) ) ;
#20058 = CARTESIAN_POINT ( 'NONE',  ( 0.02190250779246093876, -0.3346456692913385988, 1.953740157480315043 ) ) ;
#20059 = EDGE_CURVE ( 'NONE', #9665, #26728, #16976, .T. ) ;
#20060 = DIRECTION ( 'NONE',  ( 0.000000000000000000, 0.000000000000000000, 1.000000000000000000 ) ) ;
#20061 = CARTESIAN_POINT ( 'NONE',  ( -0.3082037322256093170, 0.3663931537939284500, 0.1920935997048431876 ) ) ;
#20062 = AXIS2_PLACEMENT_3D ( 'NONE', #21336, #25705, #25284 ) ;
#20063 = DIRECTION ( 'NONE',  ( 0.000000000000000000, -1.000000000000000000, 0.000000000000000000 ) ) ;
#20064 = CARTESIAN_POINT ( 'NONE',  ( 0.2577577458591218673, -0.4472135058506043759, 1.766732283464566899 ) ) ;
#20065 = AXIS2_PLACEMENT_3D ( 'NONE', #3758, #23422, #5899 ) ;
#20066 = CARTESIAN_POINT ( 'NONE',  ( -0.1293227632562458651, -0.3543012242648960752, 0.07637630750536809898 ) ) ;
#20067 = ORIENTED_EDGE ( 'NONE', *, *, #5984, .F. ) ;
#20068 = DIRECTION ( 'NONE',  ( 0.000000000000000000, 0.000000000000000000, 1.000000000000000000 ) ) ;
#20069 = ORIENTED_EDGE ( 'NONE', *, *, #11730, .F. ) ;
#20070 = CARTESIAN_POINT ( 'NONE',  ( -0.4537304931026616139, 0.07942646906834205378, 0.1771653543307086243 ) ) ;
#20071 = ( REPRESENTATION_RELATIONSHIP ('NONE','NONE', #12434, #9188 ) REPRESENTATION_RELATIONSHIP_WITH_TRANSFORMATION ( #32 )SHAPE_REPRESENTATION_RELATIONSHIP( ) ) ;
#20072 = CARTESIAN_POINT ( 'NONE',  ( -0.3135473077061334268, 0.000000000000000000, 2.504921259842519898 ) ) ;
#20073 = CARTESIAN_POINT ( 'NONE',  ( 2.632951206231566310, -0.4724409448818898127, -0.8182917201112815953 ) ) ;
#20074 = EDGE_LOOP ( 'NONE', ( #22800, #26923, #22163, #19863, #25575, #803, #6212, #22584, #14491, #10916, #14691, #4378, #10447, #26805 ) ) ;
#20075 = B_SPLINE_CURVE_WITH_KNOTS ( 'NONE', 3,
 ( #11609, #20230, #890, #9621, #16143, #24740 ),
 .UNSPECIFIED., .F., .F.,
 ( 4, 2, 4 ),
 ( 0.2291966065698869959, 0.2305109203526899964, 0.2318252341354939960 ),
 .UNSPECIFIED. ) ;
#20076 = CARTESIAN_POINT ( 'NONE',  ( 0.000000000000000000, 0.000000000000000000, 0.2362204724409449064 ) ) ;
#20077 = EDGE_LOOP ( 'NONE', ( #1725, #9676, #4747, #3926, #1372, #11602 ) ) ;
#20078 = AXIS2_PLACEMENT_3D ( 'NONE', #21852, #9822, #1762 ) ;
#20079 = PLANE ( 'NONE',  #24313 ) ;
#20080 = CIRCLE ( 'NONE', #7917, 0.5007874015748031704 ) ;
#20081 = CARTESIAN_POINT ( 'NONE',  ( 0.7872492035923605025, 0.3024535499017155238, -0.1268920345179428144 ) ) ;
#20082 = CARTESIAN_POINT ( 'NONE',  ( -0.4055118110236220486, -0.4724409448818898127, -0.9491381768041949885 ) ) ;
#20083 = EDGE_LOOP ( 'NONE', ( #10096, #9748 ) ) ;
#20084 = FACE_OUTER_BOUND ( 'NONE', #4107, .T. ) ;
#20085 = CARTESIAN_POINT ( 'NONE',  ( 0.4270824798167666692, -0.2466292688015215839, -1.550196850393700920 ) ) ;
#20086 = EDGE_CURVE ( 'NONE', #11989, #3374, #17425, .T. ) ;
#20087 = VECTOR ( 'NONE', #1382, 39.37007874015748143 ) ;
#20088 = CARTESIAN_POINT ( 'NONE',  ( 0.000000000000000000, 0.07874015748031495954, 0.000000000000000000 ) ) ;
#20089 = CARTESIAN_POINT ( 'NONE',  ( -0.3030032861724965554, -0.3454440660767394422, -1.928289503579165620 ) ) ;
#20090 = CARTESIAN_POINT ( 'NONE',  ( -0.4055118110236220486, 0.9448818897637796255, -9.561468503937007847E-18 ) ) ;
#20091 = DIRECTION ( 'NONE',  ( 0.000000000000000000, 0.000000000000000000, -1.000000000000000000 ) ) ;
#20092 = CARTESIAN_POINT ( 'NONE',  ( 0.0004974201395668345887, 0.3464563358313496044, 0.1478915661244618873 ) ) ;
#20093 = DIRECTION ( 'NONE',  ( 0.000000000000000000, 1.000000000000000000, 0.000000000000000000 ) ) ;
#20094 = CARTESIAN_POINT ( 'NONE',  ( 0.3218517393631780688, 0.3826375019114283682, 0.1259302777232058079 ) ) ;
#20095 = B_SPLINE_CURVE_WITH_KNOTS ( 'NONE', 3,
 ( #1392, #8050, #8184, #10012, #25832, #10566 ),
 .UNSPECIFIED., .F., .F.,
 ( 4, 2, 4 ),
 ( 0.000000000000000000, 0.2500000000000000000, 0.5000000000000000000 ),
 .UNSPECIFIED. ) ;
#20096 = CIRCLE ( 'NONE', #7934, 0.09143349766193348271 ) ;
#20097 = CARTESIAN_POINT ( 'NONE',  ( -0.1771653543307086520, -5.663984251968503442E-18, -0.1673228346456692994 ) ) ;
#20098 = CARTESIAN_POINT ( 'NONE',  ( -0.3031496062992123375, 0.000000000000000000, -0.4566929133858267376 ) ) ;
#20099 = CARTESIAN_POINT ( 'NONE',  ( 0.4143937130606526464, 0.4928070724618983101, 0.2359405056194269767 ) ) ;
#20100 = EDGE_CURVE ( 'NONE', #20178, #18714, #4772, .T. ) ;
#20101 = CIRCLE ( 'NONE', #27333, 0.3464566929133857665 ) ;
#20102 = ( CONVERSION_BASED_UNIT ( 'INCH', #16157 ) LENGTH_UNIT ( ) NAMED_UNIT ( #389 ) ) ;
#20103 = DIRECTION ( 'NONE',  ( -0.5000000000000002220, -0.8660254037844384856, 0.000000000000000000 ) ) ;
#20104 = CARTESIAN_POINT ( 'NONE',  ( 0.000000000000000000, 0.000000000000000000, 0.3401574803149606252 ) ) ;
#20105 = AXIS2_PLACEMENT_3D ( 'NONE', #23765, #5370, #12005 ) ;
#20106 = ORIENTED_EDGE ( 'NONE', *, *, #7382, .F. ) ;
#20107 = FACE_OUTER_BOUND ( 'NONE', #26970, .T. ) ;
#20108 = ORIENTED_EDGE ( 'NONE', *, *, #11834, .T. ) ;
#20109 = CARTESIAN_POINT ( 'NONE',  ( 0.2761764805255614297, 0.3599896729929412120, -1.934055118110236338 ) ) ;
#20110 = CARTESIAN_POINT ( 'NONE',  ( 0.0006362927944354157799, 0.4836123550484514033, 0.2715646632799083582 ) ) ;
#20111 = CARTESIAN_POINT ( 'NONE',  ( -0.4932478747986535628, 0.08657132889677658649, 0.09684874903502814492 ) ) ;
#20112 = CARTESIAN_POINT ( 'NONE',  ( 0.03937007874015747977, 0.000000000000000000, -0.3346456692913385988 ) ) ;
#20113 = CARTESIAN_POINT ( 'NONE',  ( 0.03008364706454716778, 0.1136516277932338587, -0.1968503937007874127 ) ) ;
#20114 = CARTESIAN_POINT ( 'NONE',  ( 0.1490609433576163545, 0.2393035190829114200, 0.4144858534816307505 ) ) ;
#20115 = CARTESIAN_POINT ( 'NONE',  ( -0.6869867706933208140, 0.8452458407161751452, -0.05661920376100448155 ) ) ;
#20116 = DIRECTION ( 'NONE',  ( -1.000000000000000000, 0.000000000000000000, 0.000000000000000000 ) ) ;
#20117 = FACE_OUTER_BOUND ( 'NONE', #18359, .T. ) ;
#20118 = CARTESIAN_POINT ( 'NONE',  ( -0.04928467685644277035, -0.3740848232703729015, -3.100567304031765392 ) ) ;
#20119 = AXIS2_PLACEMENT_3D ( 'NONE', #11148, #24412, #19768 ) ;
#20120 = DIRECTION ( 'NONE',  ( 0.000000000000000000, 0.000000000000000000, -1.000000000000000000 ) ) ;
#20121 = CARTESIAN_POINT ( 'NONE',  ( -5.747161356628524594E-17, -0.4692913385826771866, 0.07637795275590551769 ) ) ;
#20122 = ADVANCED_FACE ( 'NONE', ( #19388 ), #4353, .T. ) ;
#20123 = ORIENTED_EDGE ( 'NONE', *, *, #8900, .F. ) ;
#20124 = EDGE_CURVE ( 'NONE', #6094, #13081, #10191, .T. ) ;
#20125 = ( BOUNDED_CURVE ( )  B_SPLINE_CURVE ( 3, ( #25603, #21506, #1723, #8231 ),
 .UNSPECIFIED., .F., .F. ) 
 B_SPLINE_CURVE_WITH_KNOTS ( ( 4, 4 ),
 ( 3.028426401679941815, 3.254758905499644417 ),
 .UNSPECIFIED. ) 
 CURVE ( )  GEOMETRIC_REPRESENTATION_ITEM ( )  RATIONAL_B_SPLINE_CURVE ( ( 1.000000000000000000, 0.9957356870045845909, 0.9957356870045845909, 1.000000000000000000 ) ) 
 REPRESENTATION_ITEM ( '' )  ) ;
#20126 = SHAPE_DEFINITION_REPRESENTATION ( #19519, #16232 ) ;
#20127 = ORIENTED_EDGE ( 'NONE', *, *, #17785, .F. ) ;
#20128 = VERTEX_POINT ( 'NONE', #6678 ) ;
#20129 = CARTESIAN_POINT ( 'NONE',  ( -0.4162944719209866196, 0.3316996361851582975, 0.1322810039474933141 ) ) ;
#20130 = DIRECTION ( 'NONE',  ( -0.9930684569432060016, 0.1175373975568611284, 0.000000000000000000 ) ) ;
#20131 = B_SPLINE_CURVE_WITH_KNOTS ( 'NONE', 3,
 ( #24130, #547, #24262, #9143, #4911, #13523 ),
 .UNSPECIFIED., .F., .F.,
 ( 4, 2, 4 ),
 ( 0.000000000000000000, 0.2500000000000000000, 0.5000000000000000000 ),
 .UNSPECIFIED. ) ;
#20132 = CARTESIAN_POINT ( 'NONE',  ( 0.4600326175560603970, 0.2268096725222477072, 1.747047244094488194 ) ) ;
#20133 = FILL_AREA_STYLE ('',( #9675 ) ) ;
#20134 = ORIENTED_EDGE ( 'NONE', *, *, #12525, .F. ) ;
#20135 = ORIENTED_EDGE ( 'NONE', *, *, #21724, .T. ) ;
#20136 = CARTESIAN_POINT ( 'NONE',  ( 0.3349073414797994475, -0.1651192144506243853, -3.115157480314960647 ) ) ;
#20137 = AXIS2_PLACEMENT_3D ( 'NONE', #7967, #5713, #6373 ) ;
#20138 = EDGE_LOOP ( 'NONE', ( #4624, #6129, #9247, #16365 ) ) ;
#20139 = CARTESIAN_POINT ( 'NONE',  ( 0.000000000000000000, 0.07874015746264864668, 0.000000000000000000 ) ) ;
#20140 = LINE ( 'NONE', #9384, #16868 ) ;
#20141 = EDGE_LOOP ( 'NONE', ( #2417, #6885, #10431, #3171, #17581, #22096 ) ) ;
#20142 = ORIENTED_EDGE ( 'NONE', *, *, #1850, .T. ) ;
#20143 = ORIENTED_EDGE ( 'NONE', *, *, #14676, .F. ) ;
#20144 = CARTESIAN_POINT ( 'NONE',  ( 0.1520643344662694629, -0.4930463976998556985, -0.03726710077533015864 ) ) ;
#20145 = CYLINDRICAL_SURFACE ( 'NONE', #26624, 0.8163976377952756325 ) ;
#20146 = ORIENTED_EDGE ( 'NONE', *, *, #22485, .F. ) ;
#20147 = VERTEX_POINT ( 'NONE', #25891 ) ;
#20148 = ORIENTED_EDGE ( 'NONE', *, *, #1101, .F. ) ;
#20149 = CARTESIAN_POINT ( 'NONE',  ( -0.7795729917428700917, 0.4543402377591519992, 0.1538738033641767755 ) ) ;
#20150 = FACE_OUTER_BOUND ( 'NONE', #5967, .T. ) ;
#20151 = CARTESIAN_POINT ( 'NONE',  ( 0.1755067523729419432, -0.6057501678605275997, 7.418299212598425247E-17 ) ) ;
#20152 = DIRECTION ( 'NONE',  ( 0.000000000000000000, -1.000000000000000000, 0.000000000000000000 ) ) ;
#20153 = DIRECTION ( 'NONE',  ( 0.000000000000000000, 0.000000000000000000, 1.000000000000000000 ) ) ;
#20154 = CIRCLE ( 'NONE', #15710, 0.5511811023622047445 ) ;
#20155 = CARTESIAN_POINT ( 'NONE',  ( -0.5610236220428271858, 1.122047244090071949, 1.311930826979132746E-15 ) ) ;
#20156 = AXIS2_PLACEMENT_3D ( 'NONE', #26216, #19446, #25948 ) ;
#20157 = CARTESIAN_POINT ( 'NONE',  ( -0.1685339107540412829, -0.2924088307484720706, 1.973425196850394192 ) ) ;
#20158 = DIRECTION ( 'NONE',  ( -0.4999999999999997780, -0.8660254037844388186, 0.000000000000000000 ) ) ;
#20159 = CIRCLE ( 'NONE', #6659, 0.09143349766193348271 ) ;
#20160 = CARTESIAN_POINT ( 'NONE',  ( 0.3222028160008074682, 0.3833711078595924970, 0.09684874903502814492 ) ) ;
#20161 = CARTESIAN_POINT ( 'NONE',  ( -0.06200787401574745644, 7.593774443531763034E-18, -4.209669677817527322 ) ) ;
#20162 = CARTESIAN_POINT ( 'NONE',  ( 0.000000000000000000, 0.1574803148899641958, -2.066929133858267598 ) ) ;
#20163 = CARTESIAN_POINT ( 'NONE',  ( -0.5314960629921260393, 0.03478633594543736884, 1.747047244094488194 ) ) ;
#20164 = ORIENTED_EDGE ( 'NONE', *, *, #19068, .F. ) ;
#20165 = EDGE_LOOP ( 'NONE', ( #19383, #2643, #20211, #18532 ) ) ;
#20166 = DIRECTION ( 'NONE',  ( 1.000000000000000000, 0.000000000000000000, 0.000000000000000000 ) ) ;
#20167 = ORIENTED_EDGE ( 'NONE', *, *, #12888, .T. ) ;
#20168 = ( NAMED_UNIT ( * ) PLANE_ANGLE_UNIT ( ) SI_UNIT ( $, .RADIAN. ) ) ;
#20169 = EDGE_LOOP ( 'NONE', ( #11746, #180, #8557, #7385 ) ) ;
#20170 = CARTESIAN_POINT ( 'NONE',  ( -0.4925073816775267788, 0.08623502184948558802, 0.1259302777239357518 ) ) ;
#20171 = ORIENTED_EDGE ( 'NONE', *, *, #55, .F. ) ;
#20172 = EDGE_CURVE ( 'NONE', #10563, #18599, #1641, .T. ) ;
#20173 = EDGE_LOOP ( 'NONE', ( #26085, #3639, #14840, #20312, #5016, #7159, #19347, #8277, #9253, #20912, #12373, #15277 ) ) ;
#20174 = CARTESIAN_POINT ( 'NONE',  ( 0.4423390553432540173, 0.2180862235769270852, -1.569881889763779625 ) ) ;
#20175 = CARTESIAN_POINT ( 'NONE',  ( -0.3430989538742943989, 0.06100393589344793588, 0.1166443193847512133 ) ) ;
#20176 = AXIS2_PLACEMENT_3D ( 'NONE', #14183, #14036, #18665 ) ;
#20177 = AXIS2_PLACEMENT_3D ( 'NONE', #2734, #17847, #1067 ) ;
#20178 = VERTEX_POINT ( 'NONE', #11049 ) ;
#20179 = CARTESIAN_POINT ( 'NONE',  ( -0.1775991818008371415, -0.5230301363771194811, 0.9399606299212598381 ) ) ;
#20180 = VERTEX_POINT ( 'NONE', #26292 ) ;
#20181 = EDGE_CURVE ( 'NONE', #27011, #23082, #27813, .T. ) ;
#20182 = DIRECTION ( 'NONE',  ( 0.000000000000000000, 0.000000000000000000, 1.000000000000000000 ) ) ;
#20183 = CARTESIAN_POINT ( 'NONE',  ( 0.1294857240059045234, -0.3542416573274181357, 0.07637795275590551769 ) ) ;
#20184 = CIRCLE ( 'NONE', #8028, 0.1181102362204720091 ) ;
#20185 = CONTEXT_DEPENDENT_SHAPE_REPRESENTATION ( #22428, #11622 ) ;
#20186 = EDGE_CURVE ( 'NONE', #12161, #24074, #216, .T. ) ;
#20187 = DIRECTION ( 'NONE',  ( 1.000000000000000000, 0.000000000000000000, 0.000000000000000000 ) ) ;
#20188 = DIRECTION ( 'NONE',  ( 0.000000000000000000, 1.000000000000000000, 0.000000000000000000 ) ) ;
#20189 = DIRECTION ( 'NONE',  ( 0.000000000000000000, 0.000000000000000000, 1.000000000000000000 ) ) ;
#20190 = DIRECTION ( 'NONE',  ( 0.000000000000000000, 0.000000000000000000, -1.000000000000000000 ) ) ;
#20191 = CARTESIAN_POINT ( 'NONE',  ( -0.3916295560398582176, 0.3131429078174728931, 0.3080453759636629374 ) ) ;
#20192 = FACE_OUTER_BOUND ( 'NONE', #11260, .T. ) ;
#20193 = CARTESIAN_POINT ( 'NONE',  ( -0.1078280746903930304, -0.3175540113612211890, 1.953740157480315043 ) ) ;
#20194 = EDGE_LOOP ( 'NONE', ( #2529, #20773 ) ) ;
#20195 = CARTESIAN_POINT ( 'NONE',  ( -0.09842519685039370636, -5.111401574803149519E-18, 0.000000000000000000 ) ) ;
#20196 = DIRECTION ( 'NONE',  ( -1.000000000000000000, 0.000000000000000000, 0.000000000000000000 ) ) ;
#20197 = DIRECTION ( 'NONE',  ( 0.000000000000000000, 0.000000000000000000, 1.000000000000000000 ) ) ;
#20198 = CYLINDRICAL_SURFACE ( 'NONE', #19342, 0.1082677165354330312 ) ;
#20199 = CARTESIAN_POINT ( 'NONE',  ( 0.4015002836606120229, -0.2311469024250759063, 0.1494804572046649349 ) ) ;
#20200 = AXIS2_PLACEMENT_3D ( 'NONE', #11637, #26748, #7544 ) ;
#20201 = DIRECTION ( 'NONE',  ( 0.3420201433256691570, 0.9396926207859084279, -0.000000000000000000 ) ) ;
#20202 = PRODUCT_DEFINITION_SHAPE ( 'NONE', 'NONE',  #27894 ) ;
#20203 = DIRECTION ( 'NONE',  ( -0.000000000000000000, 1.000000000000000000, -0.000000000000000000 ) ) ;
#20204 = LINE ( 'NONE', #8309, #10229 ) ;
#20205 = AXIS2_PLACEMENT_3D ( 'NONE', #8077, #19078, #12449 ) ;
#20206 = VERTEX_POINT ( 'NONE', #14901 ) ;
#20207 = EDGE_CURVE ( 'NONE', #23369, #9720, #3408, .T. ) ;
#20208 = DIRECTION ( 'NONE',  ( 0.000000000000000000, 1.000000000000000000, 0.000000000000000000 ) ) ;
#20209 = DIRECTION ( 'NONE',  ( 0.000000000000000000, 0.000000000000000000, 1.000000000000000000 ) ) ;
#20210 = CARTESIAN_POINT ( 'NONE',  ( -0.08600259748439401108, 0.1968503937007873850, -3.597797143241373785 ) ) ;
#20211 = ORIENTED_EDGE ( 'NONE', *, *, #20729, .F. ) ;
#20212 = EDGE_CURVE ( 'NONE', #804, #12664, #12746, .T. ) ;
#20213 = CARTESIAN_POINT ( 'NONE',  ( -0.5375739373539409893, 0.4296723508511055556, 0.1322834645669291320 ) ) ;
#20214 = ORIENTED_EDGE ( 'NONE', *, *, #21049, .F. ) ;
#20215 = CIRCLE ( 'NONE', #2605, 0.5905511811023621549 ) ;
#20216 = ORIENTED_EDGE ( 'NONE', *, *, #17921, .T. ) ;
#20217 = ( NAMED_UNIT ( * ) PLANE_ANGLE_UNIT ( ) SI_UNIT ( $, .RADIAN. ) ) ;
#20218 = AXIS2_PLACEMENT_3D ( 'NONE', #22352, #11611, #22495 ) ;
#20219 = CIRCLE ( 'NONE', #5802, 0.4692913385826771866 ) ;
#20220 = ADVANCED_FACE ( 'NONE', ( #15031 ), #19248, .F. ) ;
#20221 = COLOUR_RGB ( '', 0.72549020, 0.75294118, 0.79215686) ;
#20222 = CARTESIAN_POINT ( 'NONE',  ( 0.7872492035923605025, 0.2520782646455287379, -0.2810771231238101686 ) ) ;
#20223 = CARTESIAN_POINT ( 'NONE',  ( 0.3765118517642103146, 0.04928528614549709808, -3.100567304031763172 ) ) ;
#20224 = LINE ( 'NONE', #13864, #10964 ) ;
#20225 = EDGE_LOOP ( 'NONE', ( #2122, #9721 ) ) ;
#20226 = CIRCLE ( 'NONE', #24713, 0.5007874015748031704 ) ;
#20227 = CARTESIAN_POINT ( 'NONE',  ( -0.3175540113612294602, 0.1078280746904015375, 1.973425196850393970 ) ) ;
#20228 = CARTESIAN_POINT ( 'NONE',  ( -0.4763861460130774939, -0.1275996891957774104, -1.550196850393700920 ) ) ;
#20229 = EDGE_CURVE ( 'NONE', #27155, #12220, #21532, .T. ) ;
#20230 = CARTESIAN_POINT ( 'NONE',  ( -0.3714952424334504455, 0.06515381386493838967, 0.07637630750536809898 ) ) ;
#20231 = CARTESIAN_POINT ( 'NONE',  ( 0.4382482975805169212, -0.3362148458988646338, 0.9202755905511811330 ) ) ;
#20232 = CARTESIAN_POINT ( 'NONE',  ( 0.1220886091274603069, -0.3369140789169591255, 0.09506557083486352755 ) ) ;
#20233 = CARTESIAN_POINT ( 'NONE',  ( 0.000000000000000000, 0.000000000000000000, -6.283251968503937502E-17 ) ) ;
#20234 = CARTESIAN_POINT ( 'NONE',  ( 0.6791338582677166613, 0.5893189861902062843, 0.000000000000000000 ) ) ;
#20235 = CARTESIAN_POINT ( 'NONE',  ( 0.3765118517642104257, -2.263258471485603576E-17, -3.100567304031763172 ) ) ;
#20236 = AXIS2_PLACEMENT_3D ( 'NONE', #13254, #20027, #11408 ) ;
#20237 = AXIS2_PLACEMENT_3D ( 'NONE', #22281, #4907, #18158 ) ;
#20238 = CARTESIAN_POINT ( 'NONE',  ( 0.000000000000000000, 0.000000000000000000, -4.330708661396418080 ) ) ;
#20239 = CARTESIAN_POINT ( 'NONE',  ( 0.1516263115863346334, -0.1971492568089275588, -0.4530651079966787620 ) ) ;
#20240 = CARTESIAN_POINT ( 'NONE',  ( 0.000000000000000000, 0.000000000000000000, -0.2480314960629921295 ) ) ;
#20241 = CARTESIAN_POINT ( 'NONE',  ( 0.3220512119205940493, 0.3834984712787528061, 0.2574827755769819038 ) ) ;
#20242 = ( LENGTH_UNIT ( ) NAMED_UNIT ( * ) SI_UNIT ( $, .METRE. ) ) ;
#20243 = DIRECTION ( 'NONE',  ( 0.000000000000000000, 1.000000000000000000, 0.000000000000000000 ) ) ;
#20244 = DIRECTION ( 'NONE',  ( 0.000000000000000000, 0.000000000000000000, 1.000000000000000000 ) ) ;
#20245 = EDGE_CURVE ( 'NONE', #17596, #8851, #8632, .T. ) ;
#20246 = ORIENTED_EDGE ( 'NONE', *, *, #10729, .T. ) ;
#20247 = CARTESIAN_POINT ( 'NONE',  ( 0.3429834333089943899, 0.09193786035240139598, 1.953740157480315043 ) ) ;
#20248 = ORIENTED_EDGE ( 'NONE', *, *, #9105, .F. ) ;
#20249 = CARTESIAN_POINT ( 'NONE',  ( 0.2006393256663695779, -0.4069519308876702324, -1.934055118110236338 ) ) ;
#20250 = CARTESIAN_POINT ( 'NONE',  ( -0.1968503937007874127, -0.4724409448818898127, 0.9265594366467145848 ) ) ;
#20251 = CARTESIAN_POINT ( 'NONE',  ( -0.1599629598573265865, -0.4411872753632007926, 0.1992125984251968684 ) ) ;
#20252 = CARTESIAN_POINT ( 'NONE',  ( 0.09334108100632415583, 0.3008230085310484858, -3.240743125436765126 ) ) ;
#20253 = CARTESIAN_POINT ( 'NONE',  ( 0.000000000000000000, 0.000000000000000000, 0.1771653543307086520 ) ) ;
#20254 = DIRECTION ( 'NONE',  ( -1.000000000000000000, 0.000000000000000000, 0.000000000000000000 ) ) ;
#20255 = EDGE_CURVE ( 'NONE', #17082, #22865, #22489, .T. ) ;
#20256 = CIRCLE ( 'NONE', #20275, 0.5007874015748031704 ) ;
#20257 = CARTESIAN_POINT ( 'NONE',  ( -0.3149606299212598381, 5.303588500244442984E-17, -0.4330708661417322913 ) ) ;
#20258 = DIRECTION ( 'NONE',  ( 0.000000000000000000, 0.000000000000000000, 1.000000000000000000 ) ) ;
#20259 = CIRCLE ( 'NONE', #8096, 0.3346456692913385988 ) ;
#20260 = FACE_OUTER_BOUND ( 'NONE', #21590, .T. ) ;
#20261 = CARTESIAN_POINT ( 'NONE',  ( 0.02464264302293787262, 0.3765118517642104257, -3.100567304031763172 ) ) ;
#20262 = TOROIDAL_SURFACE ( 'NONE', #10791, 0.5610236220472440971, 0.1003937007874015908 ) ;
#20263 = CARTESIAN_POINT ( 'NONE',  ( 0.3334645669291338987, 0.000000000000000000, -1.052618110236220428 ) ) ;
#20264 = EDGE_CURVE ( 'NONE', #3213, #23387, #7016, .T. ) ;
#20265 = VERTEX_POINT ( 'NONE', #27878 ) ;
#20266 = DIRECTION ( 'NONE',  ( 0.000000000000000000, 1.000000000000000000, 0.000000000000000000 ) ) ;
#20267 = AXIS2_PLACEMENT_3D ( 'NONE', #5994, #25479, #10069 ) ;
#20268 = DIRECTION ( 'NONE',  ( 0.000000000000000000, 0.000000000000000000, 1.000000000000000000 ) ) ;
#20269 = EDGE_LOOP ( 'NONE', ( #19324, #14344 ) ) ;
#20270 = ORIENTED_EDGE ( 'NONE', *, *, #15822, .T. ) ;
#20271 = CARTESIAN_POINT ( 'NONE',  ( -0.3861436020174326966, -0.8827507391022204608, -0.3410916819343109974 ) ) ;
#20272 = DIRECTION ( 'NONE',  ( 1.000000000000000000, 0.000000000000000000, 0.000000000000000000 ) ) ;
#20273 = CARTESIAN_POINT ( 'NONE',  ( 0.3121994997598087074, 0.4069448477555728250, 1.747047244094488194 ) ) ;
#20274 = ORIENTED_EDGE ( 'NONE', *, *, #13765, .F. ) ;
#20275 = AXIS2_PLACEMENT_3D ( 'NONE', #6644, #15272, #23882 ) ;
#20276 = EDGE_LOOP ( 'NONE', ( #25998, #16970, #22909, #10906 ) ) ;
#20277 = EDGE_CURVE ( 'NONE', #22878, #12620, #22944, .T. ) ;
#20278 = AXIS2_PLACEMENT_3D ( 'NONE', #19984, #9369, #13208 ) ;
#20279 = CARTESIAN_POINT ( 'NONE',  ( -0.09660931395005439848, 0.3606853515406323596, -3.115157480314960647 ) ) ;
#20280 = ORIENTED_EDGE ( 'NONE', *, *, #9385, .T. ) ;
#20281 = CARTESIAN_POINT ( 'NONE',  ( 0.7874015748031496509, 0.3931603432736094361, 0.1747896609116821598 ) ) ;
#20282 = CARTESIAN_POINT ( 'NONE',  ( 0.5190862322091315262, -0.1177929122753177127, 0.1322834645669291320 ) ) ;
#20283 = EDGE_CURVE ( 'NONE', #12499, #18597, #22029, .T. ) ;
#20284 = VERTEX_POINT ( 'NONE', #12884 ) ;
#20285 = ORIENTED_EDGE ( 'NONE', *, *, #18141, .T. ) ;
#20286 = ADVANCED_FACE ( 'NONE', ( #21517 ), #10770, .F. ) ;
#20287 = CARTESIAN_POINT ( 'NONE',  ( -0.5177165354330708347, -0.4724409448818898127, -0.8182917201112815953 ) ) ;
#20288 = CARTESIAN_POINT ( 'NONE',  ( 0.000000000000000000, 0.000000000000000000, 0.02362204724409448786 ) ) ;
#20289 = ORIENTED_EDGE ( 'NONE', *, *, #25423, .T. ) ;
#20290 = VERTEX_POINT ( 'NONE', #22473 ) ;
#20291 = CARTESIAN_POINT ( 'NONE',  ( -0.07874015748031495954, -0.04546065111729338803, -0.3779527559055118058 ) ) ;
#20292 = CARTESIAN_POINT ( 'NONE',  ( -0.3460635936744770880, 0.09269288654273796779, -3.115157480314960647 ) ) ;
#20293 = CARTESIAN_POINT ( 'NONE',  ( -0.3105958729529787465, -0.6467467715328735212, 0.3122824329333658833 ) ) ;
#20294 = DIRECTION ( 'NONE',  ( 1.000000000000000000, 0.000000000000000000, 0.000000000000000000 ) ) ;
#20295 = CARTESIAN_POINT ( 'NONE',  ( 0.4307823082429378392, 5.275561749190223172E-17, -0.1559029880880275776 ) ) ;
#20296 = DIRECTION ( 'NONE',  ( 1.000000000000000000, 0.000000000000000000, 0.000000000000000000 ) ) ;
#20297 = DIRECTION ( 'NONE',  ( 0.3420201433256691015, -0.9396926207859082059, 0.000000000000000000 ) ) ;
#20298 = AXIS2_PLACEMENT_3D ( 'NONE', #22167, #7329, #6929 ) ;
#20299 = VECTOR ( 'NONE', #17484, 39.37007874015748143 ) ;
#20300 = DIRECTION ( 'NONE',  ( -1.000000000000000000, 0.000000000000000000, 0.000000000000000000 ) ) ;
#20301 = PLANE ( 'NONE',  #22709 ) ;
#20302 = CARTESIAN_POINT ( 'NONE',  ( -0.4067073728345788064, -0.2341441294389334793, 0.1992125984251968684 ) ) ;
#20303 = CARTESIAN_POINT ( 'NONE',  ( 0.4930758245789425009, 0.08754571829529310401, 0.09685039370078740717 ) ) ;
#20304 = CARTESIAN_POINT ( 'NONE',  ( -0.3520466617656973218, 0.04638120790932954290, 1.953740157480315043 ) ) ;
#20305 = CARTESIAN_POINT ( 'NONE',  ( 0.1599629598573824862, -0.4411872753631803090, 0.07637795275590551769 ) ) ;
#20306 = CIRCLE ( 'NONE', #23932, 0.5511811023268710086 ) ;
#20307 = DIRECTION ( 'NONE',  ( 0.000000000000000000, 0.000000000000000000, -1.000000000000000000 ) ) ;
#20308 = DIRECTION ( 'NONE',  ( 0.1736481776669313581, 0.9848077530122080203, 0.000000000000000000 ) ) ;
#20309 = CARTESIAN_POINT ( 'NONE',  ( -0.4612490782034865955, 0.2663596103035612561, 1.747047244094488194 ) ) ;
#20310 = CARTESIAN_POINT ( 'NONE',  ( -0.2268096725222462362, 0.4600326175560554565, 1.766732283464566899 ) ) ;
#20311 = DIRECTION ( 'NONE',  ( -1.000000000000000000, 0.000000000000000000, 4.051737956723259176E-18 ) ) ;
#20312 = ORIENTED_EDGE ( 'NONE', *, *, #25428, .T. ) ;
#20313 = EDGE_CURVE ( 'NONE', #3232, #5851, #18352, .T. ) ;
#20314 = CYLINDRICAL_SURFACE ( 'NONE', #25517, 0.5905511811023621549 ) ;
#20315 = CARTESIAN_POINT ( 'NONE',  ( 0.2647715730835492609, -0.5498038367121063086, 0.1062972440944881941 ) ) ;
#20316 = CARTESIAN_POINT ( 'NONE',  ( -0.2669917830071097953, -0.2341095169845849866, 1.953740157480314821 ) ) ;
#20317 = ADVANCED_FACE ( 'NONE', ( #22616 ), #1009, .F. ) ;
#20318 = ORIENTED_EDGE ( 'NONE', *, *, #7468, .F. ) ;
#20319 = CARTESIAN_POINT ( 'NONE',  ( 0.000000000000000000, 0.000000000000000000, 0.2362204724409449064 ) ) ;
#20320 = EDGE_LOOP ( 'NONE', ( #15944, #21002, #27600, #14068 ) ) ;
#20321 = AXIS2_PLACEMENT_3D ( 'NONE', #1094, #7027, #22134 ) ;
#20322 = CARTESIAN_POINT ( 'NONE',  ( 0.2180862235769582824, 0.4423390553432410832, -1.569881889763779625 ) ) ;
#20323 = ORIENTED_EDGE ( 'NONE', *, *, #18548, .T. ) ;
#20324 = CARTESIAN_POINT ( 'NONE',  ( -0.2762247810519084523, -0.4783323773986298266, 0.9399606299212598381 ) ) ;
#20325 = ORIENTED_EDGE ( 'NONE', *, *, #25653, .F. ) ;
#20326 = ORIENTED_EDGE ( 'NONE', *, *, #23027, .F. ) ;
#20327 = DIRECTION ( 'NONE',  ( 0.8660254037844382635, -0.5000000000000005551, 0.000000000000000000 ) ) ;
#20328 = CIRCLE ( 'NONE', #27564, 0.4330708661417322913 ) ;
#20329 = FACE_OUTER_BOUND ( 'NONE', #11337, .T. ) ;
#20330 = B_SPLINE_CURVE_WITH_KNOTS ( 'NONE', 3,
 ( #10630, #27459, #14632, #3560, #12192, #20814 ),
 .UNSPECIFIED., .F., .F.,
 ( 4, 2, 4 ),
 ( 0.2376120521391529850, 0.2390783382518550104, 0.2405446243645580073 ),
 .UNSPECIFIED. ) ;
#20331 = ITEM_DEFINED_TRANSFORMATION ( 'NONE', 'NONE', #787,  #11588 ) ;
#20332 = CARTESIAN_POINT ( 'NONE',  ( 0.000000000000000000, -1.533249767903113305E-16, 0.000000000000000000 ) ) ;
#20333 = DIRECTION ( 'NONE',  ( 1.000000000000000000, 0.000000000000000000, 0.000000000000000000 ) ) ;
#20334 = CARTESIAN_POINT ( 'NONE',  ( -0.3458446900868161200, 0.000000000000000000, -0.2204724409448818867 ) ) ;
#20335 = DIRECTION ( 'NONE',  ( 0.000000000000000000, 0.000000000000000000, 1.000000000000000000 ) ) ;
#20336 = CARTESIAN_POINT ( 'NONE',  ( -0.05118110236220472370, -0.7539370078740157410, 9.233065434516462138E-17 ) ) ;
#20337 = CARTESIAN_POINT ( 'NONE',  ( 0.003937007874015826907, -4.406857903543305967E-18, -0.09842519685039370636 ) ) ;
#20338 = CARTESIAN_POINT ( 'NONE',  ( 0.3324885138898230341, -0.04380447413659129680, 1.953740157480315043 ) ) ;
#20339 = ADVANCED_FACE ( 'NONE', ( #15704 ), #20494, .T. ) ;
#20340 = B_SPLINE_CURVE_WITH_KNOTS ( 'NONE', 2,
 ( #26935, #24384, #1359 ),
 .UNSPECIFIED., .F., .F.,
 ( 3, 3 ),
 ( 0.000000000000000000, 1.000000000000000000 ),
 .UNSPECIFIED. ) ;
#20341 = UNCERTAINTY_MEASURE_WITH_UNIT (LENGTH_MEASURE( 1.000000000000000082E-05 ), #21616, 'distance_accuracy_value', 'NONE') ;
#20342 = ORIENTED_EDGE ( 'NONE', *, *, #21703, .F. ) ;
#20343 = EDGE_CURVE ( 'NONE', #15069, #22294, #2960, .T. ) ;
#20344 = CARTESIAN_POINT ( 'NONE',  ( -0.1477428134820414352, -0.4351030398461918081, -1.928289503579139641 ) ) ;
#20345 = VECTOR ( 'NONE', #121, 39.37007874015748854 ) ;
#20346 = DIRECTION ( 'NONE',  ( 1.000000000000000000, 0.000000000000000000, 0.000000000000000000 ) ) ;
#20347 = DIRECTION ( 'NONE',  ( -1.000000000000000000, 0.000000000000000000, 0.000000000000000000 ) ) ;
#20348 = PLANE ( 'NONE',  #19148 ) ;
#20349 = FACE_OUTER_BOUND ( 'NONE', #16260, .T. ) ;
#20350 = ORIENTED_EDGE ( 'NONE', *, *, #26796, .F. ) ;
#20351 = DIRECTION ( 'NONE',  ( 0.000000000000000000, -1.000000000000000000, 0.000000000000000000 ) ) ;
#20352 = AXIS2_PLACEMENT_3D ( 'NONE', #5772, #1518, #3775 ) ;
#20353 = EDGE_CURVE ( 'NONE', #372, #17537, #26698, .T. ) ;
#20354 = EDGE_CURVE ( 'NONE', #1869, #27489, #16168, .T. ) ;
#20355 = ORIENTED_EDGE ( 'NONE', *, *, #25903, .F. ) ;
#20356 = DIRECTION ( 'NONE',  ( 1.000000000000000000, 0.000000000000000000, 0.000000000000000000 ) ) ;
#20357 = DIRECTION ( 'NONE',  ( 0.000000000000000000, -1.000000000000000000, 0.000000000000000000 ) ) ;
#20358 = DIRECTION ( 'NONE',  ( 0.000000000000000000, 0.000000000000000000, 1.000000000000000000 ) ) ;
#20359 = ORIENTED_EDGE ( 'NONE', *, *, #11599, .F. ) ;
#20360 = CARTESIAN_POINT ( 'NONE',  ( 0.4333973147258542991, -0.2509079296564015737, 0.2574803149606298969 ) ) ;
#20361 = VECTOR ( 'NONE', #18541, 39.37007874015748143 ) ;
#20362 = CARTESIAN_POINT ( 'NONE',  ( -0.4055118110236220486, -0.4724409448818898127, 0.9491381768041928790 ) ) ;
#20363 = DIRECTION ( 'NONE',  ( 0.000000000000000000, -1.000000000000000000, 0.000000000000000000 ) ) ;
#20364 = ORIENTED_EDGE ( 'NONE', *, *, #10067, .F. ) ;
#20365 = ORIENTED_EDGE ( 'NONE', *, *, #8694, .T. ) ;
#20366 = CARTESIAN_POINT ( 'NONE',  ( -0.08676778863011193332, -0.3239425792934405024, 1.973425196850393970 ) ) ;
#20367 = CARTESIAN_POINT ( 'NONE',  ( -0.3252100150720236837, -0.3707612262533185321, -1.550196850393700920 ) ) ;
#20368 = CARTESIAN_POINT ( 'NONE',  ( -0.3031496062992123375, 0.000000000000000000, -0.4448818897637791814 ) ) ;
#20369 = ADVANCED_FACE ( 'NONE', ( #22053, #14004 ), #13569, .T. ) ;
#20370 = FACE_OUTER_BOUND ( 'NONE', #7799, .T. ) ;
#20371 = CARTESIAN_POINT ( 'NONE',  ( -0.5476281405333500718, 0.07214854559197644845, 0.9399606299212598381 ) ) ;
#20372 = FACE_OUTER_BOUND ( 'NONE', #5029, .T. ) ;
#20373 = EDGE_CURVE ( 'NONE', #935, #16738, #18395, .T. ) ;
#20374 = CARTESIAN_POINT ( 'NONE',  ( -0.1968503937007874127, 5.332515748031495785E-18, 0.09092130223458683158 ) ) ;
#20375 = EDGE_LOOP ( 'NONE', ( #14247, #25385 ) ) ;
#20376 = CARTESIAN_POINT ( 'NONE',  ( 0.6299212598425196763, 7.714310545810098438E-17, -0.006889763779527558960 ) ) ;
#20377 = EDGE_CURVE ( 'NONE', #6124, #7423, #20226, .T. ) ;
#20378 = CIRCLE ( 'NONE', #25814, 0.2952755905511810774 ) ;
#20379 = ORIENTED_EDGE ( 'NONE', *, *, #12493, .T. ) ;
#20380 = ADVANCED_FACE ( 'NONE', ( #7498 ), #26423, .T. ) ;
#20381 = DIRECTION ( 'NONE',  ( 1.000000000000000000, 0.000000000000000000, 0.000000000000000000 ) ) ;
#20382 = CARTESIAN_POINT ( 'NONE',  ( -0.7874015748031496509, 5.862181872755905604E-06, -1.869015748010449007 ) ) ;
#20383 = CARTESIAN_POINT ( 'NONE',  ( 0.01230314960629921330, 0.000000000000000000, -0.09679133858267717494 ) ) ;
#20384 = CARTESIAN_POINT ( 'NONE',  ( 0.4895462770359960136, 1.042587244177305195, -0.2949132003431571003 ) ) ;
#20385 = ORIENTED_EDGE ( 'NONE', *, *, #21647, .T. ) ;
#20386 = AXIS2_PLACEMENT_3D ( 'NONE', #11204, #4304, #21678 ) ;
#20387 = DIRECTION ( 'NONE',  ( 1.000000000000000000, 0.000000000000000000, 0.000000000000000000 ) ) ;
#20388 = DIRECTION ( 'NONE',  ( 1.000000000000000000, 0.000000000000000000, 0.000000000000000000 ) ) ;
#20389 = ORIENTED_EDGE ( 'NONE', *, *, #10995, .T. ) ;
#20390 = CARTESIAN_POINT ( 'NONE',  ( -0.2816986811832633553, 0.2161891097064990996, 1.953740157480315043 ) ) ;
#20391 = EDGE_CURVE ( 'NONE', #9781, #11452, #26990, .T. ) ;
#20392 = CARTESIAN_POINT ( 'NONE',  ( 0.000000000000000000, 0.1968503937007874127, -0.7874015748208159637 ) ) ;
#20393 = CARTESIAN_POINT ( 'NONE',  ( 0.000000000000000000, -1.707404996040164512E-16, 0.000000000000000000 ) ) ;
#20394 = CARTESIAN_POINT ( 'NONE',  ( -1.452994488188976472E-16, 0.5905905511811023745, -3.548228346456693050 ) ) ;
#20395 = DIRECTION ( 'NONE',  ( 0.000000000000000000, -0.8660254037844384856, -0.5000000000000003331 ) ) ;
#20396 = EDGE_LOOP ( 'NONE', ( #22547, #1770, #10687, #12026, #16666, #2129, #9235 ) ) ;
#20397 = DIRECTION ( 'NONE',  ( 1.000000000000000000, 0.000000000000000000, 0.000000000000000000 ) ) ;
#20398 = ORIENTED_EDGE ( 'NONE', *, *, #20995, .T. ) ;
#20399 = CARTESIAN_POINT ( 'NONE',  ( 0.000000000000000000, 0.7283464566929134243, 0.1771653543307086520 ) ) ;
#20400 = CARTESIAN_POINT ( 'NONE',  ( 0.1918813796216842782, -0.5271897577243779276, 0.2775610236220472093 ) ) ;
#20401 = ORIENTED_EDGE ( 'NONE', *, *, #18180, .F. ) ;
#20402 = CARTESIAN_POINT ( 'NONE',  ( 0.6140435224042697371, -0.4807043897637795493, 5.886930922602943265E-17 ) ) ;
#20403 = PRODUCT_DEFINITION_CONTEXT ( 'detailed design', #17906, 'design' ) ;
#20404 = ORIENTED_EDGE ( 'NONE', *, *, #20729, .T. ) ;
#20405 = CARTESIAN_POINT ( 'NONE',  ( -0.2938049579018679469, -0.3349573549949684259, -1.934055118110236338 ) ) ;
#20406 = EDGE_CURVE ( 'NONE', #15921, #17635, #14430, .T. ) ;
#20407 = TOROIDAL_SURFACE ( 'NONE', #27646, 0.4232283464566928832, 0.07677165354330708902 ) ;
#20408 = ADVANCED_FACE ( 'NONE', ( #4957 ), #22190, .F. ) ;
#20409 = APPLICATION_PROTOCOL_DEFINITION ( 'draft international standard', 'automotive_design', 1998, #24400 ) ;
#20410 = ORIENTED_EDGE ( 'NONE', *, *, #6931, .T. ) ;
#20411 = CARTESIAN_POINT ( 'NONE',  ( -0.3338887748335570560, -0.8039705855317598182, -0.9107153245080098491 ) ) ;
#20412 = CARTESIAN_POINT ( 'NONE',  ( 0.000000000000000000, 0.000000000000000000, 0.1377952755905511861 ) ) ;
#20413 = CARTESIAN_POINT ( 'NONE',  ( 0.4069448477555425714, 0.3121994997598541155, 1.747047244094488194 ) ) ;
#20414 = ORIENTED_EDGE ( 'NONE', *, *, #11461, .F. ) ;
#20415 = FACE_OUTER_BOUND ( 'NONE', #18566, .T. ) ;
#20416 = VECTOR ( 'NONE', #4848, 39.37007874015748143 ) ;
#20417 = AXIS2_PLACEMENT_3D ( 'NONE', #7976, #25195, #25058 ) ;
#20418 = EDGE_LOOP ( 'NONE', ( #26946, #10825, #22406, #20922 ) ) ;
#20419 = CARTESIAN_POINT ( 'NONE',  ( 0.3267488823401797360, -0.1886891683788832486, -3.100567304031763172 ) ) ;
#20420 = VERTEX_POINT ( 'NONE', #9317 ) ;
#20421 = CARTESIAN_POINT ( 'NONE',  ( -0.4555658499976152354, -0.06001958459474936169, -1.928289503579151187 ) ) ;
#20422 = FACE_OUTER_BOUND ( 'NONE', #17617, .T. ) ;
#20423 = ORIENTED_EDGE ( 'NONE', *, *, #23246, .F. ) ;
#20424 = ORIENTED_EDGE ( 'NONE', *, *, #18869, .F. ) ;
#20425 = AXIS2_PLACEMENT_3D ( 'NONE', #16845, #4267, #6384 ) ;
#20426 = CARTESIAN_POINT ( 'NONE',  ( -0.09842519685039370636, 0.5905905511811023745, -3.272637795275590733 ) ) ;
#20427 = CARTESIAN_POINT ( 'NONE',  ( 0.0005189969344232283309, 0.3771649972486724733, 0.1992125984251968684 ) ) ;
#20428 = CARTESIAN_POINT ( 'NONE',  ( 0.2938049579018456314, -0.3349573549949907414, -1.934055118110236338 ) ) ;
#20429 = ORIENTED_EDGE ( 'NONE', *, *, #24264, .F. ) ;
#20430 = ORIENTED_EDGE ( 'NONE', *, *, #25154, .T. ) ;
#20431 = CARTESIAN_POINT ( 'NONE',  ( 0.4986013261500205074, 6.106105181202481056E-17, -0.2204724409448818867 ) ) ;
#20432 = SPHERICAL_SURFACE ( 'NONE', #3612, 0.1003956692913385851 ) ;
#20433 = DIRECTION ( 'NONE',  ( -0.2036417511401760472, 0.9790454724845840673, -1.198985000000000095E-16 ) ) ;
#20434 = CARTESIAN_POINT ( 'NONE',  ( 0.5975837919107103158, 0.9212417737170555121, -0.1512753729487469612 ) ) ;
#20435 = CYLINDRICAL_SURFACE ( 'NONE', #6766, 0.07874015748031489015 ) ;
#20436 = PRODUCT_DEFINITION_SHAPE ( 'NONE', 'NONE',  #27899 ) ;
#20437 = AXIS2_PLACEMENT_3D ( 'NONE', #21050, #16680, #4106 ) ;
#20438 = EDGE_CURVE ( 'NONE', #10946, #18812, #8068, .T. ) ;
#20439 = AXIS2_PLACEMENT_3D ( 'NONE', #15455, #13167, #21942 ) ;
#20440 = DIRECTION ( 'NONE',  ( -0.9790454724845839563, 0.1018208755700880236, -0.1763589297585420324 ) ) ;
#20441 = CARTESIAN_POINT ( 'NONE',  ( 0.5189874374926378708, -0.1182276436463391700, 0.3401599409343964431 ) ) ;
#20442 = CARTESIAN_POINT ( 'NONE',  ( 0.1775730735577447927, -0.3074993854542728555, 1.953740157480315043 ) ) ;
#20443 = EDGE_CURVE ( 'NONE', #22315, #25524, #4315, .T. ) ;
#20444 = ORIENTED_EDGE ( 'NONE', *, *, #241, .F. ) ;
#20445 = CARTESIAN_POINT ( 'NONE',  ( 0.5905511811023621549, 0.000000000000000000, 0.000000000000000000 ) ) ;
#20446 = CARTESIAN_POINT ( 'NONE',  ( 0.3215969074633125979, 0.3838795254899315390, 0.09684874903502814492 ) ) ;
#20447 = SPHERICAL_SURFACE ( 'NONE', #8078, 0.1003956692913385851 ) ;
#20448 = ( REPRESENTATION_RELATIONSHIP ('NONE','NONE', #12434, #16232 ) REPRESENTATION_RELATIONSHIP_WITH_TRANSFORMATION ( #7903 )SHAPE_REPRESENTATION_RELATIONSHIP( ) ) ;
#20449 = AXIS2_PLACEMENT_3D ( 'NONE', #2267, #24160, #15295 ) ;
#20450 = DIRECTION ( 'NONE',  ( -0.2036417511401760472, -0.9790454724845840673, 0.000000000000000000 ) ) ;
#20451 = CARTESIAN_POINT ( 'NONE',  ( -0.2663596103035690277, -0.4612490782034817105, 1.747047244094488194 ) ) ;
#20452 = APPLICATION_CONTEXT ( 'automotive_design' ) ;
#20453 = CARTESIAN_POINT ( 'NONE',  ( -0.3382184156732009339, -0.3855916753051547574, 1.766732283464566899 ) ) ;
#20454 = ORIENTED_EDGE ( 'NONE', *, *, #22252, .F. ) ;
#20455 = EDGE_LOOP ( 'NONE', ( #3548, #25498 ) ) ;
#20456 = CARTESIAN_POINT ( 'NONE',  ( 0.000000000000000000, 0.4724409448818896462, 1.377952755905512472 ) ) ;
#20457 = ORIENTED_EDGE ( 'NONE', *, *, #22158, .F. ) ;
#20458 = DIRECTION ( 'NONE',  ( 0.2225209339563153921, 0.9749279121818232863, 0.000000000000000000 ) ) ;
#20459 = CARTESIAN_POINT ( 'NONE',  ( -0.2712027394948746117, 0.3535065162672773043, -1.934055118110236338 ) ) ;
#20460 = AXIS2_PLACEMENT_3D ( 'NONE', #24743, #21707, #26867 ) ;
#20461 = CARTESIAN_POINT ( 'NONE',  ( 0.3324885138898233672, 0.04380447413659172701, 1.973425196850393970 ) ) ;
#20462 = ORIENTED_EDGE ( 'NONE', *, *, #17978, .F. ) ;
#20463 = ORIENTED_EDGE ( 'NONE', *, *, #16639, .T. ) ;
#20464 = AXIS2_PLACEMENT_3D ( 'NONE', #3670, #10166, #8354 ) ;
#20465 = CARTESIAN_POINT ( 'NONE',  ( 0.4763861460130341396, -0.1275996891957698887, -1.569881889763779625 ) ) ;
#20466 = CARTESIAN_POINT ( 'NONE',  ( 0.4335958738490826581, -0.2505647196907697105, 0.09684793308443523374 ) ) ;
#20467 = ORIENTED_EDGE ( 'NONE', *, *, #25561, .F. ) ;
#20468 = ORIENTED_EDGE ( 'NONE', *, *, #15081, .T. ) ;
#20469 = CIRCLE ( 'NONE', #8302, 0.6212598425196850238 ) ;
#20470 = CONTEXT_DEPENDENT_SHAPE_REPRESENTATION ( #19004, #15918 ) ;
#20471 = FACE_OUTER_BOUND ( 'NONE', #12188, .T. ) ;
#20472 = CIRCLE ( 'NONE', #227, 0.09679133858267717494 ) ;
#20473 = CARTESIAN_POINT ( 'NONE',  ( 0.3339160553493882300, 1.241955529277656956, -0.7081600496628898123 ) ) ;
#20474 = DIRECTION ( 'NONE',  ( -1.000000000000000000, 0.000000000000000000, -0.000000000000000000 ) ) ;
#20475 = CARTESIAN_POINT ( 'NONE',  ( 1.197070535079588716, 0.07874015748031491790, 1.197070535079588716 ) ) ;
#20476 = DIRECTION ( 'NONE',  ( 1.000000000000000000, 0.000000000000000000, 0.000000000000000000 ) ) ;
#20477 = CARTESIAN_POINT ( 'NONE',  ( -0.2211428102655801364, -0.2521176338356625468, 1.953740157480315043 ) ) ;
#20478 = EDGE_CURVE ( 'NONE', #3247, #20609, #22750, .T. ) ;
#20479 = AXIS2_PLACEMENT_3D ( 'NONE', #18199, #24432, #22463 ) ;
#20480 = ORIENTED_EDGE ( 'NONE', *, *, #11568, .T. ) ;
#20481 = CARTESIAN_POINT ( 'NONE',  ( 0.5869493968219645641, 0.000000000000000000, 0.000000000000000000 ) ) ;
#20482 = DIRECTION ( 'NONE',  ( 0.000000000000000000, -1.000000000000000000, 0.000000000000000000 ) ) ;
#20483 = DIRECTION ( 'NONE',  ( 0.000000000000000000, 1.000000000000000000, 0.000000000000000000 ) ) ;
#20484 = DIRECTION ( 'NONE',  ( 0.000000000000000000, 0.000000000000000000, 1.000000000000000000 ) ) ;
#20485 = DIRECTION ( 'NONE',  ( 0.000000000000000000, 1.000000000000000000, 0.000000000000000000 ) ) ;
#20486 = CARTESIAN_POINT ( 'NONE',  ( -0.3751294191746886164, 0.2999672986753446069, 0.2362204724409450174 ) ) ;
#20487 = CARTESIAN_POINT ( 'NONE',  ( 0.1504127680534924905, -0.4837205684772389880, -0.03783905811610011050 ) ) ;
#20488 = CIRCLE ( 'NONE', #643, 0.09842519685039370636 ) ;
#20489 = VERTEX_POINT ( 'NONE', #3373 ) ;
#20490 = CIRCLE ( 'NONE', #21844, 0.7874015748208159637 ) ;
#20491 = EDGE_LOOP ( 'NONE', ( #10090, #8915 ) ) ;
#20492 = ORIENTED_EDGE ( 'NONE', *, *, #8372, .T. ) ;
#20493 = FACE_OUTER_BOUND ( 'NONE', #2375, .T. ) ;
#20494 = CYLINDRICAL_SURFACE ( 'NONE', #7140, 0.8163976377952756325 ) ;
#20495 = CARTESIAN_POINT ( 'NONE',  ( -0.03965503742771055162, 0.1968503937007873850, -3.617030424444270587 ) ) ;
#20496 = ORIENTED_EDGE ( 'NONE', *, *, #20889, .F. ) ;
#20497 = VECTOR ( 'NONE', #3955, 39.37007874015748143 ) ;
#20498 = FACE_OUTER_BOUND ( 'NONE', #7972, .T. ) ;
#20499 = VERTEX_POINT ( 'NONE', #12582 ) ;
#20500 = ADVANCED_FACE ( 'NONE', ( #18495 ), #23400, .T. ) ;
#20501 = CARTESIAN_POINT ( 'NONE',  ( 0.6140435224042697371, 0.4807043897637795493, 0.000000000000000000 ) ) ;
#20502 = FACE_OUTER_BOUND ( 'NONE', #19730, .T. ) ;
#20503 = CARTESIAN_POINT ( 'NONE',  ( 0.6175000359513720394, 0.5713135641347860672, -0.4682461283617597170 ) ) ;
#20504 = CONICAL_SURFACE ( 'NONE', #11465, 0.3937007874015748254, 0.2617993874999990922 ) ;
#20505 = CARTESIAN_POINT ( 'NONE',  ( 0.000000000000000000, 0.000000000000000000, 0.7844728274238290666 ) ) ;
#20506 = ORIENTED_EDGE ( 'NONE', *, *, #20186, .F. ) ;
#20507 = DIRECTION ( 'NONE',  ( 0.000000000000000000, 0.000000000000000000, -1.000000000000000000 ) ) ;
#20508 = EDGE_CURVE ( 'NONE', #12620, #20178, #23343, .T. ) ;
#20509 = VECTOR ( 'NONE', #15213, 39.37007874015748143 ) ;
#20510 = ORIENTED_EDGE ( 'NONE', *, *, #26212, .F. ) ;
#20511 = CARTESIAN_POINT ( 'NONE',  ( 0.09333873788075952582, 0.3008237467743239413, -3.580130230456529894 ) ) ;
#20512 = CARTESIAN_POINT ( 'NONE',  ( -0.4600326175569940945, -0.2268096725200247077, -1.550196850393700920 ) ) ;
#20513 = CARTESIAN_POINT ( 'NONE',  ( -0.04593175845765267579, -4.927204724409449161E-18, 0.000000000000000000 ) ) ;
#20514 = CARTESIAN_POINT ( 'NONE',  ( 0.4382482975805264136, 0.3362148458988503674, 0.9202755905511811330 ) ) ;
#20515 = FACE_BOUND ( 'NONE', #4215, .T. ) ;
#20516 = FACE_OUTER_BOUND ( 'NONE', #7246, .T. ) ;
#20517 = LINE ( 'NONE', #1307, #219 ) ;
#20518 = ORIENTED_EDGE ( 'NONE', *, *, #26119, .T. ) ;
#20519 = CARTESIAN_POINT ( 'NONE',  ( -0.04954844419243873560, 0.06231449464215510492, -0.4660331883676340214 ) ) ;
#20520 = AXIS2_PLACEMENT_3D ( 'NONE', #3774, #12394, #4198 ) ;
#20521 = CARTESIAN_POINT ( 'NONE',  ( -0.4270824798167633385, 0.2466292688015202517, -1.569881889763779625 ) ) ;
#20522 = ORIENTED_EDGE ( 'NONE', *, *, #27592, .F. ) ;
#20523 = CARTESIAN_POINT ( 'NONE',  ( 0.1516263115863346334, -0.4909405214979283838, -0.05579628926458622684 ) ) ;
#20524 = CARTESIAN_POINT ( 'NONE',  ( -0.1711665596939558887, 0.5043892184458266259, 1.747047244094488194 ) ) ;
#20525 = PRESENTATION_STYLE_ASSIGNMENT (( #15604 ) ) ;
#20526 = CARTESIAN_POINT ( 'NONE',  ( 0.4256740239334655951, 0.5062356173693111083, 0.1616495878840815137 ) ) ;
#20527 = ORIENTED_EDGE ( 'NONE', *, *, #3621, .F. ) ;
#20528 = ADVANCED_FACE ( 'NONE', ( #26997 ), #3669, .T. ) ;
#20529 = DIRECTION ( 'NONE',  ( -0.2034031393458100578, 0.000000000000000000, -0.9790950734756401763 ) ) ;
#20530 = TOROIDAL_SURFACE ( 'NONE', #5658, 0.7883858267716535861, 0.05216535433070866590 ) ;
#20531 = SPHERICAL_SURFACE ( 'NONE', #23737, 0.1299232283464566984 ) ;
#20532 = CARTESIAN_POINT ( 'NONE',  ( 0.000000000000000000, 0.000000000000000000, 0.06614173228346456601 ) ) ;
#20533 = VERTEX_POINT ( 'NONE', #10165 ) ;
#20534 = CARTESIAN_POINT ( 'NONE',  ( 0.003937007874015826907, -4.393043307086613241E-18, -0.1023622047244094474 ) ) ;
#20535 = ORIENTED_EDGE ( 'NONE', *, *, #23347, .T. ) ;
#20536 = ADVANCED_FACE ( 'NONE', ( #12294, #7928 ), #24865, .T. ) ;
#20537 = CARTESIAN_POINT ( 'NONE',  ( -0.2006393256663304703, -0.4069519308876202168, -1.934055118110236338 ) ) ;
#20538 = DIRECTION ( 'NONE',  ( 1.000000000000000000, 0.000000000000000000, 0.000000000000000000 ) ) ;
#20539 = CARTESIAN_POINT ( 'NONE',  ( -0.4330708661417322913, 1.131889763779527547, 0.000000000000000000 ) ) ;
#20540 = CARTESIAN_POINT ( 'NONE',  ( 0.1512365935307563858, -0.2025838097703629714, 0.4452123804180691535 ) ) ;
#20541 = DIRECTION ( 'NONE',  ( 1.000000000000000000, 0.000000000000000000, 0.000000000000000000 ) ) ;
#20542 = EDGE_CURVE ( 'NONE', #21365, #11054, #2612, .T. ) ;
#20543 = VERTEX_POINT ( 'NONE', #27419 ) ;
#20544 = CIRCLE ( 'NONE', #16483, 0.1299232283464566984 ) ;
#20545 = DIRECTION ( 'NONE',  ( -0.000000000000000000, 1.000000000000000000, -0.000000000000000000 ) ) ;
#20546 = FACE_BOUND ( 'NONE', #27228, .T. ) ;
#20547 = CARTESIAN_POINT ( 'NONE',  ( -0.2836590635674511307, -0.2488091035917043836, -3.100567304031761395 ) ) ;
#20548 = EDGE_CURVE ( 'NONE', #15380, #10350, #12444, .T. ) ;
#20549 = CARTESIAN_POINT ( 'NONE',  ( 0.1791101711252919282, -0.3102827802123563905, -3.115157480314960203 ) ) ;
#20550 = CARTESIAN_POINT ( 'NONE',  ( -0.0006568023596628692071, 0.5148705051073217964, 0.1473214333214610816 ) ) ;
#20551 = ORIENTED_EDGE ( 'NONE', *, *, #18603, .T. ) ;
#20552 = CARTESIAN_POINT ( 'NONE',  ( -0.4296318976990082805, 0.1458850421962457622, -1.934055118110236338 ) ) ;
#20553 = VECTOR ( 'NONE', #19799, 39.37007874015748143 ) ;
#20554 = CARTESIAN_POINT ( 'NONE',  ( -0.4498374011143459472, -0.05926487674658267174, -1.934055118110236338 ) ) ;
#20555 = CONICAL_SURFACE ( 'NONE', #5682, 0.04546065111729338803, 1.047197549999998811 ) ;
#20556 = VERTEX_POINT ( 'NONE', #3521 ) ;
#20557 = ORIENTED_EDGE ( 'NONE', *, *, #23502, .F. ) ;
#20558 = CARTESIAN_POINT ( 'NONE',  ( 0.5501272682988856966, 0.4396946356861675120, 0.1443310008633659491 ) ) ;
#20559 = CARTESIAN_POINT ( 'NONE',  ( 0.5118110236220472231, -0.03349795313260760937, 1.747047244094488194 ) ) ;
#20560 = AXIS2_PLACEMENT_3D ( 'NONE', #14653, #25353, #12913 ) ;
#20561 = ORIENTED_EDGE ( 'NONE', *, *, #11302, .T. ) ;
#20562 = CARTESIAN_POINT ( 'NONE',  ( 0.000000000000000000, 0.000000000000000000, -0.1464516454673935042 ) ) ;
#20563 = ORIENTED_EDGE ( 'NONE', *, *, #2477, .F. ) ;
#20564 = B_SPLINE_CURVE_WITH_KNOTS ( 'NONE', 3,
 ( #8963, #4720, #9224, #6584, #13074, #6859, #6076, #15210 ),
 .UNSPECIFIED., .F., .F.,
 ( 4, 2, 2, 4 ),
 ( 0.000000000000000000, 0.1250000000000001943, 0.2500000000000003886, 0.5000000000000000000 ),
 .UNSPECIFIED. ) ;
#20565 = EDGE_CURVE ( 'NONE', #12967, #19645, #19440, .T. ) ;
#20566 = CARTESIAN_POINT ( 'NONE',  ( -0.09762295995069376897, -0.3644697409450285974, -3.100567304031760951 ) ) ;
#20567 = VERTEX_POINT ( 'NONE', #25293 ) ;
#20568 = CARTESIAN_POINT ( 'NONE',  ( -0.3713448905834433322, 0.06600512665679449109, 0.07637795275590551769 ) ) ;
#20569 = DIRECTION ( 'NONE',  ( 0.000000000000000000, 1.000000000000000000, 0.000000000000000000 ) ) ;
#20570 = VERTEX_POINT ( 'NONE', #27142 ) ;
#20571 = EDGE_CURVE ( 'NONE', #20570, #14972, #25642, .T. ) ;
#20572 = CARTESIAN_POINT ( 'NONE',  ( -0.4312654560679679561, -0.5223570883078585414, -0.4252037497070341177 ) ) ;
#20573 = DIRECTION ( 'NONE',  ( 0.000000000000000000, 0.000000000000000000, -1.000000000000000000 ) ) ;
#20574 = AXIS2_PLACEMENT_3D ( 'NONE', #12019, #9894, #18494 ) ;
#20575 = ORIENTED_EDGE ( 'NONE', *, *, #15280, .F. ) ;
#20576 = VERTEX_POINT ( 'NONE', #8072 ) ;
#20577 = DIRECTION ( 'NONE',  ( -1.000000000000000000, 0.000000000000000000, 0.000000000000000000 ) ) ;
#20578 = EDGE_CURVE ( 'NONE', #19729, #25584, #16684, .T. ) ;
#20579 = AXIS2_PLACEMENT_3D ( 'NONE', #26026, #2423, #13158 ) ;
#20580 = B_SPLINE_CURVE_WITH_KNOTS ( 'NONE', 3,
 ( #4779, #2384, #555, #2658, #20170, #9280, #19639, #21754, #17892, #22293 ),
 .UNSPECIFIED., .F., .F.,
 ( 4, 2, 2, 2, 4 ),
 ( 0.000000000000000000, 0.2500000000000000000, 0.5000000000000000000, 0.7500000000000000000, 1.000000000000000000 ),
 .UNSPECIFIED. ) ;
#20581 = CARTESIAN_POINT ( 'NONE',  ( 0.1151913129404385921, 0.3392387706403768299, -3.115157480314960647 ) ) ;
#20582 = DIRECTION ( 'NONE',  ( 1.000000000000000000, 0.000000000000000000, 0.000000000000000000 ) ) ;
#20583 = CARTESIAN_POINT ( 'NONE',  ( 0.000000000000000000, 0.1968503937007874127, 0.000000000000000000 ) ) ;
#20584 = CARTESIAN_POINT ( 'NONE',  ( 0.5257397301587535265, 1.004902120442729085, -0.2449955022150021589 ) ) ;
#20585 = CARTESIAN_POINT ( 'NONE',  ( 0.1522836969815822838, 0.1970374587168192970, 0.4531137400420984229 ) ) ;
#20586 = CARTESIAN_POINT ( 'NONE',  ( 0.1518453843511950729, -0.1971119371026653633, -0.4530813475000614599 ) ) ;
#20587 = EDGE_CURVE ( 'NONE', #7118, #22055, #5812, .T. ) ;
#20588 = DIRECTION ( 'NONE',  ( 1.000000000000000000, 0.000000000000000000, 0.000000000000000000 ) ) ;
#20589 = PRODUCT_DEFINITION_FORMATION_WITH_SPECIFIED_SOURCE ( 'ANY', '', #27628, .NOT_KNOWN. ) ;
#20590 = CARTESIAN_POINT ( 'NONE',  ( -0.1968503937007874127, -1.676732283464567127E-17, -0.09092130223458683158 ) ) ;
#20591 = CARTESIAN_POINT ( 'NONE',  ( -0.4055118110236220486, -0.4724409448818898127, -0.8182917201112815953 ) ) ;
#20592 = ORIENTED_EDGE ( 'NONE', *, *, #25342, .F. ) ;
#20593 = AXIS2_PLACEMENT_3D ( 'NONE', #4923, #15943, #2930 ) ;
#20594 = FACE_OUTER_BOUND ( 'NONE', #23842, .T. ) ;
#20595 = CARTESIAN_POINT ( 'NONE',  ( 0.5118110236220472231, -0.03349795313260760937, 1.747047244094488194 ) ) ;
#20596 = CARTESIAN_POINT ( 'NONE',  ( -0.2268096725222457366, -0.4600326175560556230, 1.766732283464566899 ) ) ;
#20597 = AXIS2_PLACEMENT_3D ( 'NONE', #15293, #4535, #17117 ) ;
#20598 = ORIENTED_EDGE ( 'NONE', *, *, #15688, .F. ) ;
#20599 = CARTESIAN_POINT ( 'NONE',  ( -0.3460635936744770880, 0.09269288654273796779, -3.115157480314960647 ) ) ;
#20600 = ORIENTED_EDGE ( 'NONE', *, *, #26972, .T. ) ;
#20601 = DIRECTION ( 'NONE',  ( 0.2588190449580413666, 0.000000000000000000, 0.9659258263277814560 ) ) ;
#20602 = DIRECTION ( 'NONE',  ( 1.000000000000000000, 0.000000000000000000, 0.000000000000000000 ) ) ;
#20603 = DIRECTION ( 'NONE',  ( 0.000000000000000000, 0.000000000000000000, -1.000000000000000000 ) ) ;
#20604 = EDGE_LOOP ( 'NONE', ( #13360, #26147, #20463, #12232 ) ) ;
#20605 = EDGE_LOOP ( 'NONE', ( #12039, #25398, #9653, #18650, #19643, #6238 ) ) ;
#20606 = EDGE_CURVE ( 'NONE', #15892, #25182, #12150, .T. ) ;
#20607 = CARTESIAN_POINT ( 'NONE',  ( 0.3001918266902277588, 0.3912931228432131592, -1.569881889763779625 ) ) ;
#20608 = ORIENTED_EDGE ( 'NONE', *, *, #17104, .F. ) ;
#20609 = VERTEX_POINT ( 'NONE', #18636 ) ;
#20610 = ORIENTED_EDGE ( 'NONE', *, *, #10132, .T. ) ;
#20611 = EDGE_CURVE ( 'NONE', #25295, #13542, #24278, .T. ) ;
#20612 = AXIS2_PLACEMENT_3D ( 'NONE', #20615, #10146, #16379 ) ;
#20613 = TOROIDAL_SURFACE ( 'NONE', #8434, 0.5610236220472440971, 0.1003937007874015908 ) ;
#20614 = CARTESIAN_POINT ( 'NONE',  ( 0.000000000000000000, 0.000000000000000000, 0.1377952755905511861 ) ) ;
#20615 = CARTESIAN_POINT ( 'NONE',  ( 0.003937007874015826907, -4.393043307086613241E-18, 0.000000000000000000 ) ) ;
#20616 = DIRECTION ( 'NONE',  ( 1.000000000000000000, 0.000000000000000000, 0.000000000000000000 ) ) ;
#20617 = PRODUCT_DEFINITION_SHAPE ( 'NONE', 'NONE',  #23987 ) ;
#20618 = EDGE_CURVE ( 'NONE', #15239, #21578, #14288, .T. ) ;
#20619 = AXIS2_PLACEMENT_3D ( 'NONE', #24902, #22511, #18248 ) ;
#20620 = AXIS2_PLACEMENT_3D ( 'NONE', #21120, #10095, #8128 ) ;
#20621 = CARTESIAN_POINT ( 'NONE',  ( -0.3759206409296169116, 0.2989751379763687655, 0.2529987172502118908 ) ) ;
#20623 = EDGE_CURVE ( 'NONE', #13081, #6278, #23615, .T. ) ;
#20622 = UNCERTAINTY_MEASURE_WITH_UNIT (LENGTH_MEASURE( 1.000000000000000082E-05 ), #10223, 'distance_accuracy_value', 'NONE') ;
#20624 = DIRECTION ( 'NONE',  ( 0.000000000000000000, 1.000000000000000000, 0.000000000000000000 ) ) ;
#20625 = DIRECTION ( 'NONE',  ( -0.000000000000000000, -1.000000000000000000, -0.000000000000000000 ) ) ;
#20626 = CARTESIAN_POINT ( 'NONE',  ( -0.6346825714933396201, -0.07770321308519005654, 0.2339371447117805369 ) ) ;
#20627 = PLANE ( 'NONE',  #8962 ) ;
#20628 = CARTESIAN_POINT ( 'NONE',  ( -0.2299571666332044795, 0.2748389101983655380, 0.09506557084787936596 ) ) ;
#20629 = FACE_OUTER_BOUND ( 'NONE', #23640, .T. ) ;
#20630 = ORIENTED_EDGE ( 'NONE', *, *, #23687, .F. ) ;
#20631 = CARTESIAN_POINT ( 'NONE',  ( -0.5177165354330708347, 0.9448818897637796255, -0.1771653543307086520 ) ) ;
#20632 = ORIENTED_EDGE ( 'NONE', *, *, #26108, .F. ) ;
#20633 = VERTEX_POINT ( 'NONE', #25994 ) ;
#20634 = ADVANCED_FACE ( 'NONE', ( #27705 ), #15420, .F. ) ;
#20635 = CARTESIAN_POINT ( 'NONE',  ( -0.09842519685039370636, -0.07874015748031495954, 0.04546065111729338803 ) ) ;
#20636 = CARTESIAN_POINT ( 'NONE',  ( 0.1516263115863346334, 0.4909405214979283838, 0.05579628926458630317 ) ) ;
#20637 = CARTESIAN_POINT ( 'NONE',  ( 0.04956879678462433603, 0.2165354330708661457, -3.634230943941095138 ) ) ;
#20638 = ORIENTED_EDGE ( 'NONE', *, *, #26548, .T. ) ;
#20639 = EDGE_CURVE ( 'NONE', #11291, #2213, #22468, .T. ) ;
#20640 = CARTESIAN_POINT ( 'NONE',  ( -0.3223547283257516272, 0.3832433309296771617, 0.2574803149606298969 ) ) ;
#20641 = EDGE_LOOP ( 'NONE', ( #25265, #5019 ) ) ;
#20642 = EDGE_CURVE ( 'NONE', #21448, #2756, #26522, .T. ) ;
#20643 = CARTESIAN_POINT ( 'NONE',  ( 0.5382052855068000241, 0.4288813374988101890, 0.3401599409343964431 ) ) ;
#20644 = FACE_OUTER_BOUND ( 'NONE', #22618, .T. ) ;
#20645 = CARTESIAN_POINT ( 'NONE',  ( 1.197070535079588716, 0.07874015748031495954, -1.197070535079588716 ) ) ;
#20646 = CARTESIAN_POINT ( 'NONE',  ( -0.5708661417322835607, 0.6942509683549429322, 8.502122262008311951E-17 ) ) ;
#20647 = ORIENTED_EDGE ( 'NONE', *, *, #21256, .F. ) ;
#20648 = CIRCLE ( 'NONE', #8474, 0.3771653543307086909 ) ;
#20649 = CARTESIAN_POINT ( 'NONE',  ( -0.3334645669291338987, 1.286842404713327115, -0.9809137335991812146 ) ) ;
#20650 = CARTESIAN_POINT ( 'NONE',  ( 0.6212598425196851348, 0.000000000000000000, 0.09685039370078740717 ) ) ;
#20651 = CARTESIAN_POINT ( 'NONE',  ( -0.3387265385688507657, 0.4407612517155324872, 0.9202755905511812440 ) ) ;
#20652 = DIRECTION ( 'NONE',  ( -0.3420201433256691015, -0.9396926207859082059, 0.000000000000000000 ) ) ;
#20653 = CARTESIAN_POINT ( 'NONE',  ( 0.2762247810519017355, -0.4783323773986510319, 0.9202755905511811330 ) ) ;
#20654 = DIRECTION ( 'NONE',  ( 0.000000000000000000, 0.000000000000000000, 1.000000000000000000 ) ) ;
#20655 = CARTESIAN_POINT ( 'NONE',  ( -0.1294857240059045234, -0.3542416573274181357, 0.1992125984251968684 ) ) ;
#20656 = VERTEX_POINT ( 'NONE', #8891 ) ;
#20657 = CARTESIAN_POINT ( 'NONE',  ( -0.4157391792961063204, 0.3323952789219086768, 0.3401574803149606252 ) ) ;
#20658 = EDGE_CURVE ( 'NONE', #21309, #24096, #27540, .T. ) ;
#20659 = CARTESIAN_POINT ( 'NONE',  ( 0.4921259842519685179, 0.03220957031754003580, -1.569881889763779625 ) ) ;
#20660 = CARTESIAN_POINT ( 'NONE',  ( 0.000000000000000000, 0.7283464566929134243, 0.3425196850393700809 ) ) ;
#20661 = DIRECTION ( 'NONE',  ( -0.000000000000000000, -0.000000000000000000, -1.000000000000000000 ) ) ;
#20662 = CARTESIAN_POINT ( 'NONE',  ( 0.3197948809217066590, -0.6622502000673956557, 0.1960773254355315520 ) ) ;
#20663 = CIRCLE ( 'NONE', #7576, 0.1003956692913385851 ) ;
#20664 = ORIENTED_EDGE ( 'NONE', *, *, #767, .F. ) ;
#20665 = DIRECTION ( 'NONE',  ( 0.000000000000000000, 0.000000000000000000, 1.000000000000000000 ) ) ;
#20666 = CARTESIAN_POINT ( 'NONE',  ( 0.5905511811023621549, 0.000000000000000000, 0.9399606299212598381 ) ) ;
#20667 = TOROIDAL_SURFACE ( 'NONE', #18800, 0.6751968503937006982, 0.01377952755905511792 ) ;
#20668 = PRODUCT_DEFINITION_SHAPE ( 'NONE', 'NONE',  #27919 ) ;
#20669 = DIRECTION ( 'NONE',  ( 0.000000000000000000, 0.000000000000000000, 1.000000000000000000 ) ) ;
#20670 = CARTESIAN_POINT ( 'NONE',  ( 0.003937007874015826907, -4.393043307086613241E-18, 0.000000000000000000 ) ) ;
#20671 = ORIENTED_EDGE ( 'NONE', *, *, #1078, .T. ) ;
#20672 = CARTESIAN_POINT ( 'NONE',  ( -0.3520570504767979725, 0.04632170870437362503, 1.953740157480315043 ) ) ;
#20673 = ORIENTED_EDGE ( 'NONE', *, *, #19368, .T. ) ;
#20674 = CARTESIAN_POINT ( 'NONE',  ( -0.4783464566929133688, -0.4724409448818898127, 0.9954570744419902750 ) ) ;
#20675 = CARTESIAN_POINT ( 'NONE',  ( -0.4931450244001936989, 0.08715529520342381320, 0.09684793308443542803 ) ) ;
#20676 = CARTESIAN_POINT ( 'NONE',  ( -0.02563572372337621225, 0.3139795790815559373, -3.177391021203589183 ) ) ;
#20677 = CARTESIAN_POINT ( 'NONE',  ( -0.2362204724409449064, -0.4724409448818898127, -0.9491381768041949885 ) ) ;
#20678 = CARTESIAN_POINT ( 'NONE',  ( 0.2019525613798654196, 0.3664466487725783206, -0.6347042139374537983 ) ) ;
#20679 = EDGE_LOOP ( 'NONE', ( #20551, #16120, #6197, #16963 ) ) ;
#20680 = CARTESIAN_POINT ( 'NONE',  ( -0.2236164729188093725, 0.2672714825438527453, 0.1589462317847418760 ) ) ;
#20681 = DIRECTION ( 'NONE',  ( 0.000000000000000000, -1.000000000000000000, 0.000000000000000000 ) ) ;
#20682 = CARTESIAN_POINT ( 'NONE',  ( -0.2239856983871502394, -0.4635973202214443978, 0.1473214333416535404 ) ) ;
#20683 = CARTESIAN_POINT ( 'NONE',  ( 0.4986013261500205074, 6.106105181202481056E-17, -0.1033464566929133965 ) ) ;
#20684 = VECTOR ( 'NONE', #24944, 39.37007874015748854 ) ;
#20685 = PRODUCT_DEFINITION_CONTEXT ( 'detailed design', #12151, 'design' ) ;
#20686 = ORIENTED_EDGE ( 'NONE', *, *, #9563, .T. ) ;
#20687 = CARTESIAN_POINT ( 'NONE',  ( 0.02909913904662007542, 0.4446020952038907681, -1.934055118110236338 ) ) ;
#20688 = VECTOR ( 'NONE', #18014, 39.37007874015748143 ) ;
#20689 = TOROIDAL_SURFACE ( 'NONE', #15731, 0.7883858267716535861, 0.05216535433070866590 ) ;
#20690 = EDGE_CURVE ( 'NONE', #783, #11128, #2390, .T. ) ;
#20691 = ADVANCED_FACE ( 'NONE', ( #14873 ), #17555, .T. ) ;
#20692 = EDGE_CURVE ( 'NONE', #18664, #16453, #26122, .T. ) ;
#20693 = ORIENTED_EDGE ( 'NONE', *, *, #6586, .F. ) ;
#20694 = CARTESIAN_POINT ( 'NONE',  ( -0.3503688343903059166, -0.7354936199756122450, -0.6941598510668859356 ) ) ;
#20695 = CARTESIAN_POINT ( 'NONE',  ( -0.07874015748031495954, 0.04546065111729338803, -0.4724409448818898127 ) ) ;
#20696 = CARTESIAN_POINT ( 'NONE',  ( -0.4777261797697572310, -0.2355331214654124150, 1.747047244094488194 ) ) ;
#20697 = ADVANCED_FACE ( 'NONE', ( #315 ), #25720, .F. ) ;
#20698 = VERTEX_POINT ( 'NONE', #24007 ) ;
#20699 = ORIENTED_EDGE ( 'NONE', *, *, #24344, .T. ) ;
#20700 = SURFACE_STYLE_USAGE ( .BOTH. , #25502 ) ;
#20701 = VERTEX_POINT ( 'NONE', #26130 ) ;
#20702 = CARTESIAN_POINT ( 'NONE',  ( -0.3765118517642104257, 0.000000000000000000, -3.100567304031763172 ) ) ;
#20703 = EDGE_CURVE ( 'NONE', #14659, #17723, #23879, .T. ) ;
#20704 = CARTESIAN_POINT ( 'NONE',  ( -0.7874015748031496509, 0.3058301319751310920, -0.2956682880063846164 ) ) ;
#20705 = CARTESIAN_POINT ( 'NONE',  ( -0.5378903297326614874, 0.4292762795476984805, 0.1322810039474933141 ) ) ;
#20706 = ORIENTED_EDGE ( 'NONE', *, *, #17447, .T. ) ;
#20707 = CARTESIAN_POINT ( 'NONE',  ( -0.3509880991366251535, -0.7344191267098763021, -0.6958448607219711590 ) ) ;
#20708 = AXIS2_PLACEMENT_3D ( 'NONE', #19059, #19205, #5946 ) ;
#20709 = DIRECTION ( 'NONE',  ( 0.000000000000000000, -0.000000000000000000, -1.000000000000000000 ) ) ;
#20710 = TOROIDAL_SURFACE ( 'NONE', #12590, 0.4232283464566928832, 0.07677165354330708902 ) ;
#20711 = VERTEX_POINT ( 'NONE', #6367 ) ;
#20712 = CARTESIAN_POINT ( 'NONE',  ( 0.1970259548082107792, -0.3996230174612653285, -1.934055118110236338 ) ) ;
#20713 = EDGE_LOOP ( 'NONE', ( #26047, #18287, #3578, #24303, #26029, #16258, #11956 ) ) ;
#20714 = FACE_OUTER_BOUND ( 'NONE', #1448, .T. ) ;
#20715 = SPHERICAL_SURFACE ( 'NONE', #20784, 0.1003956692913385851 ) ;
#20716 = CARTESIAN_POINT ( 'NONE',  ( 0.1584254766472199816, -0.3213305936751578717, -3.115157480314960647 ) ) ;
#20717 = CARTESIAN_POINT ( 'NONE',  ( 0.000000000000000000, 0.000000000000000000, -0.2618110236220472231 ) ) ;
#20718 = CARTESIAN_POINT ( 'NONE',  ( 0.1685339107540412273, 0.2924088307484721816, 1.973425196850394192 ) ) ;
#20719 = CARTESIAN_POINT ( 'NONE',  ( -0.3334645669291338987, 0.9723695918681358741, -0.9984365296554585933 ) ) ;
#20720 = CARTESIAN_POINT ( 'NONE',  ( -0.7874015748031496509, 0.000000000000000000, -1.052618110236220428 ) ) ;
#20721 = B_SPLINE_CURVE_WITH_KNOTS ( 'NONE', 3,
 ( #16073, #15792, #7740, #18156, #16354, #24956 ),
 .UNSPECIFIED., .F., .F.,
 ( 4, 2, 4 ),
 ( 0.9359046326922999537, 0.9375808709372039917, 0.9392571091821070306 ),
 .UNSPECIFIED. ) ;
#20722 = DIRECTION ( 'NONE',  ( 1.000000000000000000, 0.000000000000000000, 0.000000000000000000 ) ) ;
#20723 = DIRECTION ( 'NONE',  ( 0.000000000000000000, 0.000000000000000000, -1.000000000000000000 ) ) ;
#20724 = LINE ( 'NONE', #13805, #5339 ) ;
#20725 = CARTESIAN_POINT ( 'NONE',  ( 0.3520466617656973218, -0.04638120790932973719, 1.953740157480315043 ) ) ;
#20726 = AXIS2_PLACEMENT_3D ( 'NONE', #24145, #20603, #7755 ) ;
#20727 = VERTEX_POINT ( 'NONE', #13273 ) ;
#20728 = CARTESIAN_POINT ( 'NONE',  ( -0.2860009521618332440, 0.4954734376824599384, 0.9399606299212600602 ) ) ;
#20729 = EDGE_CURVE ( 'NONE', #13827, #8922, #25206, .T. ) ;
#20730 = CARTESIAN_POINT ( 'NONE',  ( -0.4535326485287287657, 0.08054850140359764987, 0.1771653543307088186 ) ) ;
#20731 = DIRECTION ( 'NONE',  ( 0.000000000000000000, 0.000000000000000000, 1.000000000000000000 ) ) ;
#20732 = AXIS2_PLACEMENT_3D ( 'NONE', #19435, #18867, #10536 ) ;
#20733 = EDGE_CURVE ( 'NONE', #18478, #7957, #5350, .T. ) ;
#20734 = B_SPLINE_CURVE_WITH_KNOTS ( 'NONE', 3,
 ( #18657, #12603, #14757, #21224, #1306, #20794 ),
 .UNSPECIFIED., .F., .F.,
 ( 4, 2, 4 ),
 ( 0.6902184472752670441, 0.6915327610580710438, 0.6928470748408740443 ),
 .UNSPECIFIED. ) ;
#20735 = DIRECTION ( 'NONE',  ( 1.000000000000000000, 0.000000000000000000, 0.000000000000000000 ) ) ;
#20736 = CARTESIAN_POINT ( 'NONE',  ( 0.5314960629921260393, 0.000000000000000000, 1.747047244094488194 ) ) ;
#20737 = CARTESIAN_POINT ( 'NONE',  ( 0.1522836969735573143, -0.1970374587079578854, 0.4531137400369409374 ) ) ;
#20738 = ADVANCED_FACE ( 'NONE', ( #15137 ), #17535, .T. ) ;
#20739 = CARTESIAN_POINT ( 'NONE',  ( 0.1327036767659575123, -0.4954415918530866714, 1.766732283464566899 ) ) ;
#20740 = ORIENTED_EDGE ( 'NONE', *, *, #5952, .T. ) ;
#20741 = ORIENTED_EDGE ( 'NONE', *, *, #8401, .F. ) ;
#20742 = DIRECTION ( 'NONE',  ( 0.000000000000000000, 0.000000000000000000, 1.000000000000000000 ) ) ;
#20743 = ORIENTED_EDGE ( 'NONE', *, *, #23215, .F. ) ;
#20744 = ADVANCED_FACE ( 'NONE', ( #7288 ), #19769, .F. ) ;
#20745 = CARTESIAN_POINT ( 'NONE',  ( -0.7874015748031496509, 0.3943205132762559462, -0.07664873632799094894 ) ) ;
#20746 = DIRECTION ( 'NONE',  ( 1.000000000000000000, 0.000000000000000000, 0.000000000000000000 ) ) ;
#20747 = EDGE_LOOP ( 'NONE', ( #4352, #13404, #18214, #21432, #26157, #15099 ) ) ;
#20748 = ORIENTED_EDGE ( 'NONE', *, *, #15398, .F. ) ;
#20749 = CARTESIAN_POINT ( 'NONE',  ( -0.4921259842519685179, 0.000000000000000000, -1.569881889763779625 ) ) ;
#20750 = ORIENTED_EDGE ( 'NONE', *, *, #21159, .F. ) ;
#20751 = AXIS2_PLACEMENT_3D ( 'NONE', #3601, #18178, #5751 ) ;
#20752 = EDGE_CURVE ( 'NONE', #18986, #18301, #865, .T. ) ;
#20753 = AXIS2_PLACEMENT_3D ( 'NONE', #6762, #23727, #26238 ) ;
#20754 = ITEM_DEFINED_TRANSFORMATION ( 'NONE', 'NONE', #8019,  #11588 ) ;
#20755 = CARTESIAN_POINT ( 'NONE',  ( -0.4325730547867440712, 0.000000000000000000, -0.1740172276534823204 ) ) ;
#20756 = DIRECTION ( 'NONE',  ( 0.000000000000000000, 0.000000000000000000, 1.000000000000000000 ) ) ;
#20757 = CARTESIAN_POINT ( 'NONE',  ( 0.000000000000000000, 0.000000000000000000, 0.1771653543307086520 ) ) ;
#20758 = DIRECTION ( 'NONE',  ( -0.4999999999999995004, 0.8660254037844390407, 0.000000000000000000 ) ) ;
#20759 = CIRCLE ( 'NONE', #19847, 0.5511811023622047445 ) ;
#20760 = VERTEX_POINT ( 'NONE', #14226 ) ;
#20761 = DIRECTION ( 'NONE',  ( 0.000000000000000000, 0.000000000000000000, 1.000000000000000000 ) ) ;
#20762 = DIRECTION ( 'NONE',  ( 0.000000000000000000, 1.000000000000000000, 0.000000000000000000 ) ) ;
#20763 = SPHERICAL_SURFACE ( 'NONE', #16414, 0.07677362204724409722 ) ;
#20764 = ADVANCED_FACE ( 'NONE', ( #22408 ), #18425, .T. ) ;
#20765 = CARTESIAN_POINT ( 'NONE',  ( 0.5511811023622047445, 0.000000000000000000, 0.01181102362204724393 ) ) ;
#20766 = CARTESIAN_POINT ( 'NONE',  ( -0.06441914069860964209, 0.4921259842519686845, -1.569881889763779625 ) ) ;
#20767 = FACE_BOUND ( 'NONE', #25715, .T. ) ;
#20768 = EDGE_CURVE ( 'NONE', #2223, #18599, #24736, .T. ) ;
#20769 = ORIENTED_EDGE ( 'NONE', *, *, #24166, .T. ) ;
#20770 = CIRCLE ( 'NONE', #26616, 0.6212598425196850238 ) ;
#20771 = ORIENTED_EDGE ( 'NONE', *, *, #27512, .F. ) ;
#20772 = CARTESIAN_POINT ( 'NONE',  ( 0.09590060490395689585, -0.1136516277932334562, 0.1968503937007874127 ) ) ;
#20773 = ORIENTED_EDGE ( 'NONE', *, *, #14472, .T. ) ;
#20774 = ADVANCED_FACE ( 'NONE', ( #11807 ), #26929, .F. ) ;
#20775 = ORIENTED_EDGE ( 'NONE', *, *, #25343, .F. ) ;
#20776 = CIRCLE ( 'NONE', #7698, 0.1082677165354330312 ) ;
#20777 = DIRECTION ( 'NONE',  ( 1.000000000000000000, 0.000000000000000000, 0.000000000000000000 ) ) ;
#20778 = DIRECTION ( 'NONE',  ( 0.000000000000000000, -7.180547322999998243E-06, 0.9999999999742198442 ) ) ;
#20779 = DIMENSIONAL_EXPONENTS ( 1.000000000000000000, 0.000000000000000000, 0.000000000000000000, 0.000000000000000000, 0.000000000000000000, 0.000000000000000000, 0.000000000000000000 ) ;
#20780 = ORIENTED_EDGE ( 'NONE', *, *, #8111, .T. ) ;
#20781 = ORIENTED_EDGE ( 'NONE', *, *, #8518, .F. ) ;
#20782 = PLANE ( 'NONE',  #7553 ) ;
#20783 = DIRECTION ( 'NONE',  ( 0.000000000000000000, 0.000000000000000000, -1.000000000000000000 ) ) ;
#20784 = AXIS2_PLACEMENT_3D ( 'NONE', #1360, #27215, #23125 ) ;
#20785 = CARTESIAN_POINT ( 'NONE',  ( 0.3543307086614173040, -1.934043700787401319E-18, 0.000000000000000000 ) ) ;
#20786 = ORIENTED_EDGE ( 'NONE', *, *, #15845, .F. ) ;
#20787 = CARTESIAN_POINT ( 'NONE',  ( -0.6342142812942709318, 0.1111449751011379800, 0.1183902030371653535 ) ) ;
#20788 = ORIENTED_EDGE ( 'NONE', *, *, #14957, .T. ) ;
#20789 = DIRECTION ( 'NONE',  ( -0.7071067818211409506, 0.7071067805519539728, 8.659560554583403090E-17 ) ) ;
#20790 = CARTESIAN_POINT ( 'NONE',  ( 0.2775852647713619725, 0.4816145447621894005, 0.9202755905511812440 ) ) ;
#20791 = EDGE_CURVE ( 'NONE', #6332, #16370, #16183, .T. ) ;
#20792 = VECTOR ( 'NONE', #3162, 39.37007874015748854 ) ;
#20793 = CARTESIAN_POINT ( 'NONE',  ( 0.5511811023622047445, 0.03607471876262480226, 0.9202755905511811330 ) ) ;
#20794 = CARTESIAN_POINT ( 'NONE',  ( 0.2420394123212937232, 0.2892587550802425134, 0.1992125984251968684 ) ) ;
#20795 = CARTESIAN_POINT ( 'NONE',  ( 0.000000000000000000, 0.000000000000000000, -0.04133858267716535029 ) ) ;
#20796 = VERTEX_POINT ( 'NONE', #22548 ) ;
#20797 = DIRECTION ( 'NONE',  ( 0.9930684569549264040, -0.05876869872891801738, -0.1017903720931950112 ) ) ;
#20798 = EDGE_CURVE ( 'NONE', #2204, #27155, #16411, .T. ) ;
#20799 = DIRECTION ( 'NONE',  ( 1.000000000000000000, 0.000000000000000000, 0.000000000000000000 ) ) ;
#20800 = CARTESIAN_POINT ( 'NONE',  ( -0.02576258753921337533, 0.2165354330708661457, -3.176774343053047733 ) ) ;
#20801 = VERTEX_POINT ( 'NONE', #26778 ) ;
#20802 = AXIS2_PLACEMENT_3D ( 'NONE', #2057, #25652, #6310 ) ;
#20803 = DIRECTION ( 'NONE',  ( 0.000000000000000000, 0.000000000000000000, -1.000000000000000000 ) ) ;
#20804 = CARTESIAN_POINT ( 'NONE',  ( 0.3680051700917441604, 0.000000000000000000, 0.000000000000000000 ) ) ;
#20805 = DIRECTION ( 'NONE',  ( 0.000000000000000000, -1.000000000000000000, 0.000000000000000000 ) ) ;
#20806 = DIRECTION ( 'NONE',  ( 0.000000000000000000, -1.000000000000000000, 0.000000000000000000 ) ) ;
#20807 = ORIENTED_EDGE ( 'NONE', *, *, #6186, .F. ) ;
#20808 = DIRECTION ( 'NONE',  ( 0.000000000000000000, -1.000000000000000000, 0.000000000000000000 ) ) ;
#20809 = VERTEX_POINT ( 'NONE', #12087 ) ;
#20810 = CARTESIAN_POINT ( 'NONE',  ( 0.4339912984563291110, -0.2498791196563492356, 0.2574803149606298969 ) ) ;
#20811 = CARTESIAN_POINT ( 'NONE',  ( 6.026805113914139867E-17, 0.5905511811023621549, 0.4921259842519685179 ) ) ;
#20812 = CARTESIAN_POINT ( 'NONE',  ( -0.09842519685039377575, 0.2991866959364320455, -3.266083869132035744 ) ) ;
#20813 = CIRCLE ( 'NONE', #18477, 0.1181102362204720091 ) ;
#20814 = CARTESIAN_POINT ( 'NONE',  ( 0.3012109481302311376, 0.3598698725862007897, 0.07637795275590551769 ) ) ;
#20815 = CARTESIAN_POINT ( 'NONE',  ( 0.5890517850735842442, -0.1332273157280143838, -0.2362204724409449064 ) ) ;
#20816 = ORIENTED_EDGE ( 'NONE', *, *, #22959, .T. ) ;
#20817 = SURFACE_SIDE_STYLE ('',( #16443 ) ) ;
#20818 = CARTESIAN_POINT ( 'NONE',  ( 0.1522836969735572310, 0.4941010236220472751, 0.000000000000000000 ) ) ;
#20819 = DIRECTION ( 'NONE',  ( 1.000000000000000000, 0.000000000000000000, 0.000000000000000000 ) ) ;
#20820 = SURFACE_SIDE_STYLE ('',( #16314 ) ) ;
#20821 = VERTEX_POINT ( 'NONE', #7862 ) ;
#20822 = CARTESIAN_POINT ( 'NONE',  ( 0.1152775731717068236, 0.4303822302054135518, -1.934055118110236338 ) ) ;
#20823 = AXIS2_PLACEMENT_3D ( 'NONE', #23234, #4149, #25621 ) ;
#20824 = EDGE_CURVE ( 'NONE', #7632, #5599, #7664, .T. ) ;
#20825 = VECTOR ( 'NONE', #7933, 39.37007874015748143 ) ;
#20826 = AXIS2_PLACEMENT_3D ( 'NONE', #18084, #9632, #7528 ) ;
#20827 = EDGE_LOOP ( 'NONE', ( #22500, #8331 ) ) ;
#20828 = ORIENTED_EDGE ( 'NONE', *, *, #4155, .T. ) ;
#20829 = CARTESIAN_POINT ( 'NONE',  ( 0.5744851493179060631, 0.4591414886162703546, 0.1960773254404601651 ) ) ;
#20830 = SURFACE_STYLE_FILL_AREA ( #27763 ) ;
#20831 = SHAPE_DEFINITION_REPRESENTATION ( #26732, #13162 ) ;
#20832 = EDGE_LOOP ( 'NONE', ( #3306, #5378, #20365, #23809 ) ) ;
#20833 = CARTESIAN_POINT ( 'NONE',  ( 0.3991696156513551141, 0.4760540497243913594, 0.09684793308443542803 ) ) ;
#20834 = ORIENTED_EDGE ( 'NONE', *, *, #20018, .F. ) ;
#20835 = CARTESIAN_POINT ( 'NONE',  ( -0.1886891683788859964, 0.3267488823401775155, -3.100567304031764948 ) ) ;
#20836 = EDGE_CURVE ( 'NONE', #22837, #15321, #12788, .T. ) ;
#20837 = CARTESIAN_POINT ( 'NONE',  ( -0.1968503937007874127, 0.9793307086614173596, 0.000000000000000000 ) ) ;
#20838 = B_SPLINE_SURFACE_WITH_KNOTS ( 'NONE', 3, 3, ( 
 ( #1332, #16440, #20815, #27187 ),
 ( #12339, #25053, #16574, #16171 ),
 ( #1462, #5716, #7693, #18679 ),
 ( #1602, #5857, #20960, #27461 ) ),
 .UNSPECIFIED., .F., .F., .F.,
 ( 4, 4 ),
 ( 4, 4 ),
 ( -1.199999999999999956, 0.000000000000000000 ),
 ( -5.261281292110230545, -3.749855894370889953 ),
 .UNSPECIFIED. ) ;
#20839 = DIRECTION ( 'NONE',  ( -1.000000000000000000, 0.000000000000000000, 0.000000000000000000 ) ) ;
#20840 = CARTESIAN_POINT ( 'NONE',  ( -0.04638120790932972332, -0.3520466617656973218, 1.953740157480315043 ) ) ;
#20841 = ORIENTED_EDGE ( 'NONE', *, *, #22731, .T. ) ;
#20842 = AXIS2_PLACEMENT_3D ( 'NONE', #6274, #8522, #8792 ) ;
#20843 = CARTESIAN_POINT ( 'NONE',  ( -0.5816775848650642677, -0.1674846703394633762, -0.2535625474260125856 ) ) ;
#20845 = CARTESIAN_POINT ( 'NONE',  ( -0.4954156765914823346, 0.2860899518036844058, 0.9399606299212598381 ) ) ;
#20844 = CARTESIAN_POINT ( 'NONE',  ( -0.03532354024591771724, -1.259842519685039353, 7.714310545810098438E-17 ) ) ;
#20846 = DIRECTION ( 'NONE',  ( 0.1736481776669300814, -0.9848077530122080203, 0.000000000000000000 ) ) ;
#20847 = EDGE_LOOP ( 'NONE', ( #24612, #25532 ) ) ;
#20848 = EDGE_LOOP ( 'NONE', ( #20496, #6211 ) ) ;
#20849 = DIRECTION ( 'NONE',  ( -0.9930684569549264040, 0.05876869872891801738, -0.1017903720931950112 ) ) ;
#20850 = CARTESIAN_POINT ( 'NONE',  ( 0.000000000000000000, 0.000000000000000000, 0.2574803149606298969 ) ) ;
#20851 = AXIS2_PLACEMENT_3D ( 'NONE', #15329, #26174, #12307 ) ;
#20852 = EDGE_CURVE ( 'NONE', #26151, #26623, #5828, .T. ) ;
#20853 = CONICAL_SURFACE ( 'NONE', #7776, 0.2362204724225640262, 0.2617993875000002579 ) ;
#20854 = CARTESIAN_POINT ( 'NONE',  ( -0.3460635936744816399, -0.09269288654274071559, -3.115157480314960647 ) ) ;
#20855 = CARTESIAN_POINT ( 'NONE',  ( -0.4771018889076559244, 0.3804760601893846794, 0.2362204724409449064 ) ) ;
#20856 = DIRECTION ( 'NONE',  ( 0.000000000000000000, -1.000000000000000000, 0.000000000000000000 ) ) ;
#20857 = CARTESIAN_POINT ( 'NONE',  ( -0.3334645669291338987, 1.286842404713327115, -0.9809137335991812146 ) ) ;
#20858 = CIRCLE ( 'NONE', #18578, 1.131889763779527547 ) ;
#20859 = DIRECTION ( 'NONE',  ( 0.000000000000000000, 0.000000000000000000, -1.000000000000000000 ) ) ;
#20860 = ADVANCED_FACE ( 'NONE', ( #23264, #12513 ), #1771, .T. ) ;
#20861 = CARTESIAN_POINT ( 'NONE',  ( -0.07874015748031495954, 5.303588500244442984E-17, -0.4330708661417322913 ) ) ;
#20862 = TOROIDAL_SURFACE ( 'NONE', #14117, 0.3722026523000413478, 0.02755905511811023584 ) ;
#20863 = EDGE_LOOP ( 'NONE', ( #10835, #14055, #5247, #20671, #6499 ) ) ;
#20864 = DIRECTION ( 'NONE',  ( 0.000000000000000000, 0.000000000000000000, 1.000000000000000000 ) ) ;
#20865 = CONICAL_SURFACE ( 'NONE', #3697, 0.6942509683549429322, 0.2617993875000015902 ) ;
#20867 = DIRECTION ( 'NONE',  ( 1.000000000000000000, 0.000000000000000000, 0.000000000000000000 ) ) ;
#20866 = CIRCLE ( 'NONE', #6904, 0.3937007874015748254 ) ;
#20868 = CARTESIAN_POINT ( 'NONE',  ( 0.7378141273707626846, -0.5132596510569377157, 0.1342805930655029401 ) ) ;
#20869 = CARTESIAN_POINT ( 'NONE',  ( 0.5314960629921260393, -0.03478633594540021801, 1.747047244094488194 ) ) ;
#20870 = PRODUCT_CONTEXT ( 'NONE', #19550, 'mechanical' ) ;
#20871 = CARTESIAN_POINT ( 'NONE',  ( -0.09842519685039366473, 0.1968503937007873850, -3.272637795275590733 ) ) ;
#20872 = CARTESIAN_POINT ( 'NONE',  ( 0.5118110236220472231, 0.000000000000000000, 1.747047244094488194 ) ) ;
#20873 = ORIENTED_EDGE ( 'NONE', *, *, #24629, .T. ) ;
#20874 = AXIS2_PLACEMENT_3D ( 'NONE', #7265, #24092, #24361 ) ;
#20875 = B_SPLINE_CURVE_WITH_KNOTS ( 'NONE', 3,
 ( #7997, #5882, #25076, #23112, #21124, #14511 ),
 .UNSPECIFIED., .F., .F.,
 ( 4, 2, 4 ),
 ( 0.7157687286427140139, 0.7172350147555670574, 0.7187013008684189908 ),
 .UNSPECIFIED. ) ;
#20876 = VERTEX_POINT ( 'NONE', #21966 ) ;
#20877 = CARTESIAN_POINT ( 'NONE',  ( -0.3574975638436101444, 0.000000000000000000, -3.115157480314960647 ) ) ;
#20878 = ORIENTED_EDGE ( 'NONE', *, *, #2419, .F. ) ;
#20879 = CARTESIAN_POINT ( 'NONE',  ( 0.3759206409296168561, 0.2989751379763686545, 0.2194422276324867749 ) ) ;
#20880 = FACE_OUTER_BOUND ( 'NONE', #2151, .T. ) ;
#20881 = DIRECTION ( 'NONE',  ( 0.000000000000000000, 0.000000000000000000, 1.000000000000000000 ) ) ;
#20882 = VERTEX_POINT ( 'NONE', #15617 ) ;
#20883 = ORIENTED_EDGE ( 'NONE', *, *, #15702, .T. ) ;
#20884 = EDGE_CURVE ( 'NONE', #25216, #3117, #25925, .T. ) ;
#20885 = CARTESIAN_POINT ( 'NONE',  ( 0.3707612262533330205, 0.3252100150720381722, -1.550196850393700920 ) ) ;
#20886 = VERTEX_POINT ( 'NONE', #21692 ) ;
#20887 = AXIS2_PLACEMENT_3D ( 'NONE', #155, #4892, #20007 ) ;
#20888 = CARTESIAN_POINT ( 'NONE',  ( 0.3334645669291338987, -1.114423376110021513, -0.8575999861807854785 ) ) ;
#20889 = EDGE_CURVE ( 'NONE', #10900, #17397, #23425, .T. ) ;
#20890 = AXIS2_PLACEMENT_3D ( 'NONE', #22729, #20616, #23026 ) ;
#20891 = ADVANCED_FACE ( 'NONE', ( #23814 ), #19428, .F. ) ;
#20892 = FACE_OUTER_BOUND ( 'NONE', #2103, .T. ) ;
#20893 = EDGE_CURVE ( 'NONE', #23520, #22723, #27479, .T. ) ;
#20894 = CARTESIAN_POINT ( 'NONE',  ( -0.2428345617565149384, 0.2885915454824177218, 0.1992125984251968684 ) ) ;
#20895 = CARTESIAN_POINT ( 'NONE',  ( 0.0006615832605804723319, 0.6212594902576319411, 0.2574803149606298969 ) ) ;
#20896 = EDGE_CURVE ( 'NONE', #17275, #16233, #15738, .T. ) ;
#20897 = CIRCLE ( 'NONE', #8714, 0.4980314960629921295 ) ;
#20898 = VERTEX_POINT ( 'NONE', #19975 ) ;
#20899 = DIRECTION ( 'NONE',  ( 0.000000000000000000, 0.000000000000000000, 1.000000000000000000 ) ) ;
#20900 = ADVANCED_FACE ( 'NONE', ( #22094 ), #631, .T. ) ;
#20901 = UNCERTAINTY_MEASURE_WITH_UNIT (LENGTH_MEASURE( 1.000000000000000082E-05 ), #1336, 'distance_accuracy_value', 'NONE') ;
#20902 = CARTESIAN_POINT ( 'NONE',  ( 0.000000000000000000, 0.000000000000000000, -3.110236220451535694 ) ) ;
#20903 = DIRECTION ( 'NONE',  ( 1.000000000000000000, 0.000000000000000000, 0.000000000000000000 ) ) ;
#20904 = DIRECTION ( 'NONE',  ( 0.000000000000000000, 0.000000000000000000, 1.000000000000000000 ) ) ;
#20905 = CARTESIAN_POINT ( 'NONE',  ( -0.4703564121420970578, -0.6731208498009066954, 0.04710847534168485784 ) ) ;
#20906 = CARTESIAN_POINT ( 'NONE',  ( -0.5905511811023621549, 0.000000000000000000, 0.000000000000000000 ) ) ;
#20907 = CARTESIAN_POINT ( 'NONE',  ( -0.03532354024591775193, -0.6299212598425196763, 0.000000000000000000 ) ) ;
#20908 = DIRECTION ( 'NONE',  ( 0.1736481776669313581, 0.9848077530122080203, 0.000000000000000000 ) ) ;
#20909 = AXIS2_PLACEMENT_3D ( 'NONE', #18077, #7377, #15851 ) ;
#20910 = AXIS2_PLACEMENT_3D ( 'NONE', #5097, #7098, #13719 ) ;
#20911 = ORIENTED_EDGE ( 'NONE', *, *, #22305, .F. ) ;
#20912 = ORIENTED_EDGE ( 'NONE', *, *, #7229, .F. ) ;
#20913 = CARTESIAN_POINT ( 'NONE',  ( 0.000000000000000000, 0.000000000000000000, 0.1377952755905511861 ) ) ;
#20914 = ORIENTED_EDGE ( 'NONE', *, *, #13636, .T. ) ;
#20915 = VECTOR ( 'NONE', #24531, 39.37007874015748143 ) ;
#20916 = CARTESIAN_POINT ( 'NONE',  ( -0.6117062799105453808, 0.1085321106658580781, 0.09685039370078740717 ) ) ;
#20917 = CARTESIAN_POINT ( 'NONE',  ( -0.3119936278821711650, -0.6460736482326152608, 0.1601585119449864536 ) ) ;
#20918 = AXIS2_PLACEMENT_3D ( 'NONE', #9441, #9302, #19922 ) ;
#20919 = DIRECTION ( 'NONE',  ( -1.000000000000000000, 0.000000000000000000, 0.000000000000000000 ) ) ;
#20920 = VERTEX_POINT ( 'NONE', #10948 ) ;
#20921 = FACE_OUTER_BOUND ( 'NONE', #19518, .T. ) ;
#20922 = ORIENTED_EDGE ( 'NONE', *, *, #16818, .T. ) ;
#20923 = ADVANCED_FACE ( 'NONE', ( #21547 ), #10810, .F. ) ;
#20924 = DIRECTION ( 'NONE',  ( -1.000000000000000000, 0.000000000000000000, 0.000000000000000000 ) ) ;
#20925 = DIRECTION ( 'NONE',  ( 1.000000000000000000, 0.000000000000000000, 0.000000000000000000 ) ) ;
#20926 = CARTESIAN_POINT ( 'NONE',  ( -0.4167985568850881561, 0.07349283109919312051, 0.2145688976377952695 ) ) ;
#20927 = EDGE_CURVE ( 'NONE', #10221, #3239, #17707, .T. ) ;
#20928 = TOROIDAL_SURFACE ( 'NONE', #6958, 0.4055118110236220486, 0.01181102362204724393 ) ;
#20929 = DIRECTION ( 'NONE',  ( -1.224646799147353207E-16, 1.000000000000000000, 0.000000000000000000 ) ) ;
#20930 = ORIENTED_EDGE ( 'NONE', *, *, #20373, .T. ) ;
#20931 = DIRECTION ( 'NONE',  ( 1.000000000000000000, 0.000000000000000000, 0.000000000000000000 ) ) ;
#20932 = ORIENTED_EDGE ( 'NONE', *, *, #20100, .T. ) ;
#20933 = CARTESIAN_POINT ( 'NONE',  ( 0.2521176338356670432, 0.2211428102655656758, 1.953740157480315043 ) ) ;
#20934 = DIRECTION ( 'NONE',  ( 0.000000000000000000, 0.000000000000000000, 1.000000000000000000 ) ) ;
#20935 = CIRCLE ( 'NONE', #17772, 0.7283464566929134243 ) ;
#20936 = CARTESIAN_POINT ( 'NONE',  ( -0.4382482975804890546, -0.3362148458988509225, 0.9399606299212598381 ) ) ;
#20937 = AXIS2_PLACEMENT_3D ( 'NONE', #1828, #7775, #8337 ) ;
#20938 = DIRECTION ( 'NONE',  ( 0.000000000000000000, 0.000000000000000000, 1.000000000000000000 ) ) ;
#20939 = CARTESIAN_POINT ( 'NONE',  ( 0.6106000000000000316, 0.09842519683305382683, 1.205361022570475770E-17 ) ) ;
#20940 = ADVANCED_FACE ( 'NONE', ( #17841 ), #13460, .T. ) ;
#20941 = AXIS2_PLACEMENT_3D ( 'NONE', #22147, #4769, #8877 ) ;
#20942 = EDGE_LOOP ( 'NONE', ( #8718, #9716, #19615, #19839 ) ) ;
#20943 = ORIENTED_EDGE ( 'NONE', *, *, #22676, .T. ) ;
#20944 = CARTESIAN_POINT ( 'NONE',  ( 0.8549722296228741136, -0.6488494047548032384, 1.633858267716535639 ) ) ;
#20945 = DIRECTION ( 'NONE',  ( 0.000000000000000000, 0.000000000000000000, -1.000000000000000000 ) ) ;
#20946 = CARTESIAN_POINT ( 'NONE',  ( 0.6791338582677166613, 0.000000000000000000, 0.000000000000000000 ) ) ;
#20947 = CARTESIAN_POINT ( 'NONE',  ( -0.1968503937007874127, 0.000000000000000000, 0.000000000000000000 ) ) ;
#20948 = ORIENTED_EDGE ( 'NONE', *, *, #27506, .T. ) ;
#20949 = CARTESIAN_POINT ( 'NONE',  ( -0.0007856387884314780523, 0.7354206117097525919, 0.1960773254409858557 ) ) ;
#20950 = ORIENTED_EDGE ( 'NONE', *, *, #7954, .F. ) ;
#20952 = EDGE_CURVE ( 'NONE', #17815, #4811, #1606, .T. ) ;
#20951 = AXIS2_PLACEMENT_3D ( 'NONE', #26251, #8746, #11279 ) ;
#20953 = CARTESIAN_POINT ( 'NONE',  ( 0.4771018889076559244, 0.3804760601893846794, 0.1062972440944881941 ) ) ;
#20955 = EDGE_CURVE ( 'NONE', #16432, #15505, #10011, .T. ) ;
#20954 = CARTESIAN_POINT ( 'NONE',  ( -0.5609635780474857558, -0.5548708040265607488, -0.9753554781212179225 ) ) ;
#20956 = AXIS2_PLACEMENT_3D ( 'NONE', #21033, #19191, #21321 ) ;
#20957 = CARTESIAN_POINT ( 'NONE',  ( 0.000000000000000000, 0.000000000000000000, -0.1464516454673935042 ) ) ;
#20958 = DIRECTION ( 'NONE',  ( -1.000000000000000000, 0.000000000000000000, 0.000000000000000000 ) ) ;
#20959 = ORIENTED_EDGE ( 'NONE', *, *, #2545, .T. ) ;
#20960 = CARTESIAN_POINT ( 'NONE',  ( 0.5890517850735842442, -0.2103245977542082534, 0.2362204724409449064 ) ) ;
#20961 = ADVANCED_FACE ( 'NONE', ( #13067 ), #2319, .F. ) ;
#20962 = ORIENTED_EDGE ( 'NONE', *, *, #25470, .T. ) ;
#20963 = DIRECTION ( 'NONE',  ( 1.000000000000000000, 0.000000000000000000, 0.000000000000000000 ) ) ;
#20964 = DIRECTION ( 'NONE',  ( -0.9575713608335526539, -0.1440981340193014659, 0.2495852893972990150 ) ) ;
#20965 = ORIENTED_EDGE ( 'NONE', *, *, #18711, .F. ) ;
#20966 = ( NAMED_UNIT ( * ) SI_UNIT ( $, .STERADIAN. ) SOLID_ANGLE_UNIT ( ) ) ;
#20967 = CARTESIAN_POINT ( 'NONE',  ( 0.03220957031753916844, -0.4921259842519686289, -1.569881889763779625 ) ) ;
#20968 = AXIS2_PLACEMENT_3D ( 'NONE', #25140, #1277, #22604 ) ;
#20969 = EDGE_LOOP ( 'NONE', ( #2931, #7895, #19282, #22635 ) ) ;
#20970 = CARTESIAN_POINT ( 'NONE',  ( 0.05819755867304853003, -0.4417361510194242613, -1.934055118110236338 ) ) ;
#20971 = EDGE_CURVE ( 'NONE', #13428, #7191, #13197, .T. ) ;
#20972 = CIRCLE ( 'NONE', #17368, 0.4986013261500205074 ) ;
#20973 = ORIENTED_EDGE ( 'NONE', *, *, #27826, .T. ) ;
#20974 = AXIS2_PLACEMENT_3D ( 'NONE', #17588, #2470, #15363 ) ;
#20975 = CARTESIAN_POINT ( 'NONE',  ( -0.5935113537020059171, -0.2228995930351641841, 0.2169198626053897849 ) ) ;
#20976 = CARTESIAN_POINT ( 'NONE',  ( 0.5314960629921260393, 0.03478633594540018331, 1.747047244094488194 ) ) ;
#20977 = FILL_AREA_STYLE_COLOUR ( '', #10694 ) ;
#20978 = VERTEX_POINT ( 'NONE', #8954 ) ;
#20979 = CARTESIAN_POINT ( 'NONE',  ( 0.000000000000000000, 0.000000000000000000, 0.1992125984251968684 ) ) ;
#20980 = CARTESIAN_POINT ( 'NONE',  ( 0.000000000000000000, 0.000000000000000000, 0.4724409448818898127 ) ) ;
#20981 = CARTESIAN_POINT ( 'NONE',  ( 0.3350145293470547236, 0.2937497900413817975, -1.934055118110236338 ) ) ;
#20982 = CIRCLE ( 'NONE', #26376, 0.5322834645669292097 ) ;
#20983 = CARTESIAN_POINT ( 'NONE',  ( 0.1775730735577439323, 0.3074993854542599769, 1.953740157480315043 ) ) ;
#20984 = ORIENTED_EDGE ( 'NONE', *, *, #5093, .F. ) ;
#20985 = ORIENTED_EDGE ( 'NONE', *, *, #2973, .T. ) ;
#20986 = CARTESIAN_POINT ( 'NONE',  ( -0.6108855800013244242, -0.1027495160574083549, -0.2427121449866776470 ) ) ;
#20988 = CARTESIAN_POINT ( 'NONE',  ( 0.4954156765914486393, 0.2860899518037346989, 0.9399606299212598381 ) ) ;
#20987 = DIRECTION ( 'NONE',  ( 0.000000000000000000, 0.000000000000000000, 1.000000000000000000 ) ) ;
#20989 = ( REPRESENTATION_RELATIONSHIP ('NONE','NONE', #12434, #16232 ) REPRESENTATION_RELATIONSHIP_WITH_TRANSFORMATION ( #16797 )SHAPE_REPRESENTATION_RELATIONSHIP( ) ) ;
#20990 = VERTEX_POINT ( 'NONE', #17582 ) ;
#20991 = DIRECTION ( 'NONE',  ( 0.000000000000000000, 0.000000000000000000, 1.000000000000000000 ) ) ;
#20992 = DIRECTION ( 'NONE',  ( 0.000000000000000000, 0.000000000000000000, -1.000000000000000000 ) ) ;
#20993 = EDGE_CURVE ( 'NONE', #19062, #19453, #4900, .T. ) ;
#20994 = VECTOR ( 'NONE', #16855, 39.37007874015748143 ) ;
#20995 = EDGE_CURVE ( 'NONE', #17602, #5538, #11495, .T. ) ;
#20996 = CARTESIAN_POINT ( 'NONE',  ( 0.3551931031211519874, -0.04679574315772458415, -3.115157480314960647 ) ) ;
#20997 = AXIS2_PLACEMENT_3D ( 'NONE', #22803, #17386, #20681 ) ;
#20998 = CARTESIAN_POINT ( 'NONE',  ( 0.4816145447621895115, -0.2775852647713619170, 0.9202755905511811330 ) ) ;
#20999 = DIRECTION ( 'NONE',  ( -0.9790454724845842893, 0.1018208755700882318, 0.1763589297585410332 ) ) ;
#21000 = CARTESIAN_POINT ( 'NONE',  ( -0.1771653543307086520, 1.241643108977391477E-17, 0.1476377952755905387 ) ) ;
#21001 = CARTESIAN_POINT ( 'NONE',  ( 0.000000000000000000, 0.000000000000000000, 0.04842519685039370358 ) ) ;
#21002 = ORIENTED_EDGE ( 'NONE', *, *, #15459, .T. ) ;
#21003 = CARTESIAN_POINT ( 'NONE',  ( 0.3123213164519275664, 0.3731274149352674097, 0.09284957166392941719 ) ) ;
#21004 = DIRECTION ( 'NONE',  ( 0.000000000000000000, 1.000000000000000000, 0.000000000000000000 ) ) ;
#21005 = AXIS2_PLACEMENT_3D ( 'NONE', #26875, #27028, #24604 ) ;
#21006 = VERTEX_POINT ( 'NONE', #13611 ) ;
#21007 = CARTESIAN_POINT ( 'NONE',  ( 0.4538422614035440561, 0.3483115186079798753, 0.9399606299212601712 ) ) ;
#21008 = CARTESIAN_POINT ( 'NONE',  ( -0.4620608682196346573, 0.08206165078060512208, 0.1992125984251968684 ) ) ;
#21009 = CARTESIAN_POINT ( 'NONE',  ( 0.000000000000000000, 0.000000000000000000, -0.1559029880880275776 ) ) ;
#21010 = CARTESIAN_POINT ( 'NONE',  ( 0.7874015748031496509, 5.862181872755905604E-06, -1.869015748010449007 ) ) ;
#21011 = CARTESIAN_POINT ( 'NONE',  ( -0.4600326175560542907, 0.2268096725222489285, 1.766732283464566899 ) ) ;
#21012 = ORIENTED_EDGE ( 'NONE', *, *, #17360, .T. ) ;
#21013 = EDGE_CURVE ( 'NONE', #18475, #16503, #9648, .T. ) ;
#21014 = ORIENTED_EDGE ( 'NONE', *, *, #17947, .F. ) ;
#21015 = CARTESIAN_POINT ( 'NONE',  ( -0.1294857240059045234, -0.3542416573274181357, 0.07637795275590551769 ) ) ;
#21016 = ORIENTED_EDGE ( 'NONE', *, *, #4364, .F. ) ;
#21017 = VECTOR ( 'NONE', #7696, 39.37007874015748143 ) ;
#21018 = CARTESIAN_POINT ( 'NONE',  ( -0.4256740239345673249, 0.5062356173706242801, 0.1926811207662450509 ) ) ;
#21019 = LENGTH_MEASURE_WITH_UNIT ( LENGTH_MEASURE( 0.02539999999999999897 ), #8584 ) ;
#21020 = FACE_OUTER_BOUND ( 'NONE', #22154, .T. ) ;
#21021 = CARTESIAN_POINT ( 'NONE',  ( -0.0005189969344232283309, 0.3771649972486724733, 0.07637795275590551769 ) ) ;
#21022 = CARTESIAN_POINT ( 'NONE',  ( -0.3175540113612294602, 0.1078280746904015375, 1.973425196850393970 ) ) ;
#21023 = ORIENTED_EDGE ( 'NONE', *, *, #17788, .F. ) ;
#21024 = CARTESIAN_POINT ( 'NONE',  ( -0.4889536969035060410, 0.06441834428466772233, -1.550196850393700920 ) ) ;
#21026 = EDGE_CURVE ( 'NONE', #16500, #26850, #25913, .T. ) ;
#21025 = DIRECTION ( 'NONE',  ( 1.000000000000000000, 0.000000000000000000, 0.000000000000000000 ) ) ;
#21027 = ORIENTED_EDGE ( 'NONE', *, *, #20587, .T. ) ;
#21028 = EDGE_LOOP ( 'NONE', ( #15993, #27708, #16651, #19144 ) ) ;
#21029 = ITEM_DEFINED_TRANSFORMATION ( 'NONE', 'NONE', #9347,  #11588 ) ;
#21030 = LINE ( 'NONE', #18616, #3590 ) ;
#21031 = CARTESIAN_POINT ( 'NONE',  ( 0.2131049448083992270, -0.5835666837866889667, 0.09685039370078740717 ) ) ;
#21032 = CARTESIAN_POINT ( 'NONE',  ( 0.07874015748031495954, 0.04546065111729338803, -0.3779527559055118058 ) ) ;
#21033 = CARTESIAN_POINT ( 'NONE',  ( -0.3866383478380992500, 0.000000000000000000, -0.2204724409448818867 ) ) ;
#21034 = ORIENTED_EDGE ( 'NONE', *, *, #4503, .F. ) ;
#21035 = CARTESIAN_POINT ( 'NONE',  ( -0.3785000865559329797, 0.3010298976870116050, 0.2715646632809148309 ) ) ;
#21036 = CONICAL_SURFACE ( 'NONE', #20593, 0.7122990885670630323, 0.2923426493749994304 ) ;
#21037 = CARTESIAN_POINT ( 'NONE',  ( 0.6791338582677166613, 9.401815977706058242E-17, 0.7480314960629921295 ) ) ;
#21038 = DIRECTION ( 'NONE',  ( -1.000000000000000000, 0.000000000000000000, 0.000000000000000000 ) ) ;
#21039 = DIRECTION ( 'NONE',  ( 0.000000000000000000, 1.000000000000000000, 0.000000000000000000 ) ) ;
#21040 = AXIS2_PLACEMENT_3D ( 'NONE', #9348, #24610, #1044 ) ;
#21041 = CARTESIAN_POINT ( 'NONE',  ( -0.5639365699154915701, -0.3272902772321842901, 0.1939717402340199737 ) ) ;
#21042 = LINE ( 'NONE', #18774, #13284 ) ;
#21043 = LINE ( 'NONE', #3658, #2018 ) ;
#21044 = EDGE_CURVE ( 'NONE', #27874, #401, #15088, .T. ) ;
#21045 = LINE ( 'NONE', #10446, #22196 ) ;
#21046 = VERTEX_POINT ( 'NONE', #5565 ) ;
#21047 = PRODUCT_RELATED_PRODUCT_CATEGORY ( 'part', '', ( #23113 ) ) ;
#21048 = VERTEX_POINT ( 'NONE', #20250 ) ;
#21049 = EDGE_CURVE ( 'NONE', #20633, #26083, #9400, .T. ) ;
#21050 = CARTESIAN_POINT ( 'NONE',  ( 0.000000000000000000, 0.000000000000000000, 0.01181102362204724393 ) ) ;
#21051 = ORIENTED_EDGE ( 'NONE', *, *, #2175, .T. ) ;
#21052 = AXIS2_PLACEMENT_3D ( 'NONE', #8059, #5800, #4235 ) ;
#21053 = CARTESIAN_POINT ( 'NONE',  ( -0.2362204724409449064, 0.9448818897637796255, -0.1308464566929134210 ) ) ;
#21054 = EDGE_CURVE ( 'NONE', #21624, #9806, #17955, .T. ) ;
#21055 = AXIS2_PLACEMENT_3D ( 'NONE', #7123, #24349, #17584 ) ;
#21056 = CARTESIAN_POINT ( 'NONE',  ( -0.01968503937007873988, -0.6246466694403326469, 0.000000000000000000 ) ) ;
#21057 = CARTESIAN_POINT ( 'NONE',  ( 0.1429116519061275903, 0.5335524835332325910, 0.9202755905511811330 ) ) ;
#21058 = ORIENTED_EDGE ( 'NONE', *, *, #9079, .T. ) ;
#21059 = ORIENTED_EDGE ( 'NONE', *, *, #15121, .F. ) ;
#21060 = DIRECTION ( 'NONE',  ( 0.000000000000000000, 0.000000000000000000, -1.000000000000000000 ) ) ;
#21061 = DIRECTION ( 'NONE',  ( 1.000000000000000000, 0.000000000000000000, 0.000000000000000000 ) ) ;
#21062 = DIRECTION ( 'NONE',  ( 0.000000000000000000, -7.180547322999998243E-06, 0.9999999999742198442 ) ) ;
#21063 = ORIENTED_EDGE ( 'NONE', *, *, #13984, .F. ) ;
#21064 = DIRECTION ( 'NONE',  ( 0.9848077530122080203, -0.1736481776669309973, 0.000000000000000000 ) ) ;
#21065 = ORIENTED_EDGE ( 'NONE', *, *, #25880, .T. ) ;
#21066 = CARTESIAN_POINT ( 'NONE',  ( -0.1482986320106466638, 0.3007905576423924310, 1.953740157480315043 ) ) ;
#21067 = CARTESIAN_POINT ( 'NONE',  ( 0.4441657790094322711, 0.2564944395535476707, -1.550196850393700920 ) ) ;
#21068 = CARTESIAN_POINT ( 'NONE',  ( 0.04954844419243873560, -0.06231449464215510492, -0.4660331883676339659 ) ) ;
#21069 = ADVANCED_FACE ( 'NONE', ( #26740 ), #22515, .T. ) ;
#21070 = CARTESIAN_POINT ( 'NONE',  ( 0.07214854559198032036, -0.5476281405333571772, 0.9399606299212598381 ) ) ;
#21071 = CARTESIAN_POINT ( 'NONE',  ( 2.185478346456692557E-17, -4.034314960629921845E-17, -0.1625845656552793450 ) ) ;
#21072 = EDGE_LOOP ( 'NONE', ( #9965, #6424, #9313, #10776, #16374, #5520, #14049 ) ) ;
#21073 = PRODUCT ( 'Deep Groove Ball Bearing 20x37x9', 'Deep Groove Ball Bearing 20x37x9', '', ( #20870 ) ) ;
#21074 = DIRECTION ( 'NONE',  ( 0.000000000000000000, 0.000000000000000000, 1.000000000000000000 ) ) ;
#21075 = EDGE_CURVE ( 'NONE', #17199, #19638, #2249, .T. ) ;
#21076 = ( CONVERSION_BASED_UNIT ( 'INCH', #19096 ) LENGTH_UNIT ( ) NAMED_UNIT ( #23345 ) ) ;
#21077 = ORIENTED_EDGE ( 'NONE', *, *, #6732, .T. ) ;
#21078 = PRESENTATION_LAYER_ASSIGNMENT (  '', '', ( #27853 ) ) ;
#21079 = CARTESIAN_POINT ( 'NONE',  ( -0.3242876858378660465, 0.4225410690761917665, 1.747047244094487972 ) ) ;
#21080 = B_SPLINE_CURVE_WITH_KNOTS ( 'NONE', 3,
 ( #5183, #9554, #17629, #15794, #13388, #19755, #5045, #6909 ),
 .UNSPECIFIED., .F., .F.,
 ( 4, 2, 2, 4 ),
 ( 5.336250286839431171E-07, 0.0004434172983718084209, 0.0008863009717149328238, 0.001772068318401181846 ),
 .UNSPECIFIED. ) ;
#21081 = EDGE_CURVE ( 'NONE', #22192, #26883, #26170, .T. ) ;
#21082 = ORIENTED_EDGE ( 'NONE', *, *, #17516, .T. ) ;
#21083 = CARTESIAN_POINT ( 'NONE',  ( 0.3855916753034687172, 0.3382184156749162285, -1.550196850393700920 ) ) ;
#21084 = DIRECTION ( 'NONE',  ( -0.7071067811865480168, 0.7071067811865470176, 0.000000000000000000 ) ) ;
#21085 = EDGE_CURVE ( 'NONE', #11452, #23841, #16674, .T. ) ;
#21086 = DIRECTION ( 'NONE',  ( 1.000000000000000000, 0.000000000000000000, 0.000000000000000000 ) ) ;
#21087 = DIRECTION ( 'NONE',  ( 0.000000000000000000, 0.000000000000000000, -1.000000000000000000 ) ) ;
#21088 = CARTESIAN_POINT ( 'NONE',  ( 0.000000000000000000, 0.000000000000000000, 0.1992125984251968684 ) ) ;
#21089 = EDGE_LOOP ( 'NONE', ( #24772, #5619, #7285, #25943 ) ) ;
#21090 = CARTESIAN_POINT ( 'NONE',  ( -0.0007756954652701438836, 0.7174612052774099746, 0.1601585119466828466 ) ) ;
#21091 = EDGE_LOOP ( 'NONE', ( #15865, #7033, #14950, #18745, #3413, #6226, #15834, #7844, #6707, #21341, #4730, #16723, #5460 ) ) ;
#21092 = TOROIDAL_SURFACE ( 'NONE', #21557, 0.4173228346456693272, 0.02362204724409448786 ) ;
#21093 = EDGE_CURVE ( 'NONE', #20570, #15934, #11774, .T. ) ;
#21094 = ADVANCED_FACE ( 'NONE', ( #24346 ), #24762, .T. ) ;
#21095 = DIRECTION ( 'NONE',  ( 0.000000000000000000, 0.000000000000000000, 1.000000000000000000 ) ) ;
#21096 = CARTESIAN_POINT ( 'NONE',  ( -0.5626609578937310507, -0.5839878592448841665, -0.9562163583975410441 ) ) ;
#21097 = AXIS2_PLACEMENT_3D ( 'NONE', #5417, #3550, #20529 ) ;
#21098 = AXIS2_PLACEMENT_3D ( 'NONE', #7406, #19982, #13476 ) ;
#21099 = CARTESIAN_POINT ( 'NONE',  ( 0.5869493968219645641, 0.000000000000000000, 0.000000000000000000 ) ) ;
#21100 = DIRECTION ( 'NONE',  ( -0.000000000000000000, -0.000000000000000000, -1.000000000000000000 ) ) ;
#21101 = CARTESIAN_POINT ( 'NONE',  ( 0.2239856983846744420, -0.4635973202162851914, 0.3251195115343817332 ) ) ;
#21102 = ORIENTED_EDGE ( 'NONE', *, *, #1948, .T. ) ;
#21103 = EDGE_CURVE ( 'NONE', #24815, #16432, #23831, .T. ) ;
#21104 = CARTESIAN_POINT ( 'NONE',  ( 0.3937007873768824662, 0.000000000000000000, -0.1377952755696460196 ) ) ;
#21105 = CARTESIAN_POINT ( 'NONE',  ( -0.1771653543307086520, -5.663984251968503442E-18, 0.000000000000000000 ) ) ;
#21106 = VERTEX_POINT ( 'NONE', #17003 ) ;
#21107 = CARTESIAN_POINT ( 'NONE',  ( -0.09275304139133716541, -0.3460530745557874321, -3.115157480314960647 ) ) ;
#21108 = DIRECTION ( 'NONE',  ( 0.000000000000000000, 0.000000000000000000, 1.000000000000000000 ) ) ;
#21109 = CARTESIAN_POINT ( 'NONE',  ( 0.02963280468032034737, -0.4527559054764770385, -1.934055118110236338 ) ) ;
#21110 = CARTESIAN_POINT ( 'NONE',  ( 0.3073078020556853085, 0.3671449284689711212, 0.1920935997049015298 ) ) ;
#21111 = CARTESIAN_POINT ( 'NONE',  ( -0.3645739570812708275, 0.2796934465393700053, -1.928289503579159625 ) ) ;
#21112 = CONICAL_SURFACE ( 'NONE', #27050, 1.988188976307287970, 0.7853981642948970610 ) ;
#21113 = ORIENTED_EDGE ( 'NONE', *, *, #27089, .F. ) ;
#21114 = AXIS2_PLACEMENT_3D ( 'NONE', #24916, #22808, #7548 ) ;
#21115 = CARTESIAN_POINT ( 'NONE',  ( -0.5546128944410685380, -0.3166022791122425906, 0.03369876051672000133 ) ) ;
#21116 = CARTESIAN_POINT ( 'NONE',  ( -0.5511811023622047445, 6.750021727583836750E-17, 0.2637795275590551491 ) ) ;
#21117 = CARTESIAN_POINT ( 'NONE',  ( 0.1712563538833041243, 0.5043504886477225835, 1.747047244094488194 ) ) ;
#21118 = ADVANCED_FACE ( 'NONE', ( #5852 ), #7966, .F. ) ;
#21119 = ORIENTED_EDGE ( 'NONE', *, *, #5252, .T. ) ;
#21120 = CARTESIAN_POINT ( 'NONE',  ( 0.000000000000000000, 0.000000000000000000, 0.09685039370078740717 ) ) ;
#21121 = ORIENTED_EDGE ( 'NONE', *, *, #12242, .F. ) ;
#21122 = CARTESIAN_POINT ( 'NONE',  ( -0.09842519685039370636, 0.07874015748031495954, -0.04546065111729338803 ) ) ;
#21124 = CARTESIAN_POINT ( 'NONE',  ( 0.3019498226894488102, 0.3592501948414881796, 0.1992142434433716580 ) ) ;
#21123 = AXIS2_PLACEMENT_3D ( 'NONE', #9602, #9755, #5234 ) ;
#21125 = CARTESIAN_POINT ( 'NONE',  ( -0.02917857698688259421, 0.4446006764000811629, -1.934055118110236338 ) ) ;
#21126 = EDGE_CURVE ( 'NONE', #9025, #11355, #19372, .T. ) ;
#21127 = CARTESIAN_POINT ( 'NONE',  ( 0.3074993854542699689, 0.1775730735577541186, 1.953740157480315043 ) ) ;
#21128 = ORIENTED_EDGE ( 'NONE', *, *, #10300, .T. ) ;
#21129 = CARTESIAN_POINT ( 'NONE',  ( -0.6087844546985001770, -0.1074051126585219840, -0.2433141525755926904 ) ) ;
#21130 = CYLINDRICAL_SURFACE ( 'NONE', #4547, 0.1181102362204718703 ) ;
#21131 = LINE ( 'NONE', #10386, #23021 ) ;
#21132 = ORIENTED_EDGE ( 'NONE', *, *, #19632, .F. ) ;
#21133 = CARTESIAN_POINT ( 'NONE',  ( -0.4932821129636645874, 0.08637579872942342807, 0.09685039370078740717 ) ) ;
#21134 = CARTESIAN_POINT ( 'NONE',  ( 0.3263749705684267921, -0.1890319631540330891, 0.07637795275590551769 ) ) ;
#21135 = CIRCLE ( 'NONE', #7152, 0.1771653543307086798 ) ;
#21136 = AXIS2_PLACEMENT_3D ( 'NONE', #9202, #7376, #13589 ) ;
#21137 = CARTESIAN_POINT ( 'NONE',  ( -0.2362439534887390002, -0.2693339498142257038, -3.115157480314960647 ) ) ;
#21138 = CARTESIAN_POINT ( 'NONE',  ( -0.4816145447621893450, -0.2775852647713621946, 0.9202755905511812440 ) ) ;
#21139 = VECTOR ( 'NONE', #15041, 39.37007874015748143 ) ;
#21140 = CARTESIAN_POINT ( 'NONE',  ( 1.456051859513969730E-17, 0.5007874015748032814, 0.2574827755769819038 ) ) ;
#21141 = DIRECTION ( 'NONE',  ( -0.000000000000000000, -0.000000000000000000, 1.000000000000000000 ) ) ;
#21142 = CARTESIAN_POINT ( 'NONE',  ( 0.0005963271530293720634, 0.4972008316414386897, 0.1615162260929392524 ) ) ;
#21143 = CARTESIAN_POINT ( 'NONE',  ( 0.4895462770359960136, 0.6604130065487362478, -0.5726600247964968027 ) ) ;
#21144 = DIRECTION ( 'NONE',  ( 0.000000000000000000, 0.000000000000000000, 1.000000000000000000 ) ) ;
#21145 = B_SPLINE_CURVE_WITH_KNOTS ( 'NONE', 3,
 ( #2241, #10861, #19475, #172, #6222, #14855, #23331, #23469, #10730, #14987, #19343 ),
 .UNSPECIFIED., .F., .F.,
 ( 4, 2, 1, 2, 2, 4 ),
 ( 0.5000000000000000000, 0.6249999999999993339, 0.6874999999999988898, 0.7187499999999990008, 0.7499999999999991118, 1.000000000000000000 ),
 .UNSPECIFIED. ) ;
#21146 = ORIENTED_EDGE ( 'NONE', *, *, #13667, .F. ) ;
#21147 = CARTESIAN_POINT ( 'NONE',  ( -0.3988311005573134116, 0.4763376377694984454, 0.09685039370078740717 ) ) ;
#21148 = CARTESIAN_POINT ( 'NONE',  ( 0.4301570366551352165, 0.3771675965699478050, 0.9399606299212600602 ) ) ;
#21149 = ADVANCED_FACE ( 'NONE', ( #19110 ), #12597, .F. ) ;
#21150 = CARTESIAN_POINT ( 'NONE',  ( 0.5314960629921260393, 0.000000000000000000, 1.747047244094488194 ) ) ;
#21151 = DIRECTION ( 'NONE',  ( 0.000000000000000000, 0.000000000000000000, -1.000000000000000000 ) ) ;
#21152 = DIRECTION ( 'NONE',  ( 0.000000000000000000, 1.000000000000000000, 0.000000000000000000 ) ) ;
#21153 = CARTESIAN_POINT ( 'NONE',  ( 0.2355331214654088623, -0.4777261797697378021, 1.747047244094488194 ) ) ;
#21154 = CARTESIAN_POINT ( 'NONE',  ( -0.3018020646414484309, 0.3593743330771480560, 0.07637549214372835182 ) ) ;
#21155 = CARTESIAN_POINT ( 'NONE',  ( -0.2208527687074414714, -0.6048181665966714249, 0.1183902030404290623 ) ) ;
#21156 = ADVANCED_FACE ( 'NONE', ( #25332 ), #25689, .T. ) ;
#21157 = VECTOR ( 'NONE', #4324, 39.37007874015748143 ) ;
#21158 = VERTEX_POINT ( 'NONE', #16434 ) ;
#21159 = EDGE_CURVE ( 'NONE', #1064, #14125, #22990, .T. ) ;
#21160 = ORIENTED_EDGE ( 'NONE', *, *, #4708, .T. ) ;
#21161 = AXIS2_PLACEMENT_3D ( 'NONE', #19927, #1000, #9449 ) ;
#21162 = CARTESIAN_POINT ( 'NONE',  ( 0.3392387706403792169, -0.1151913129404410208, -3.115157480314960647 ) ) ;
#21163 = VECTOR ( 'NONE', #9985, 39.37007874015748143 ) ;
#21164 = CARTESIAN_POINT ( 'NONE',  ( 0.4006498629591503380, -0.2309201403895325411, -1.928289503579156294 ) ) ;
#21165 = CARTESIAN_POINT ( 'NONE',  ( -0.2965233727166468047, 0.3524965443697193335, 0.1771653543307085965 ) ) ;
#21166 = CARTESIAN_POINT ( 'NONE',  ( 0.08676778863010879694, -0.3239425792934411685, 1.973425196850393970 ) ) ;
#21167 = ORIENTED_EDGE ( 'NONE', *, *, #23983, .F. ) ;
#21168 = ORIENTED_EDGE ( 'NONE', *, *, #22193, .T. ) ;
#21169 = CARTESIAN_POINT ( 'NONE',  ( -0.4669911931914605407, 0.1585706980422390278, -1.550196850393700920 ) ) ;
#21170 = DIRECTION ( 'NONE',  ( -0.3174974722037089969, 0.000000000000000000, -0.9482591181445370054 ) ) ;
#21171 = CIRCLE ( 'NONE', #21637, 0.4606299212598425341 ) ;
#21172 = ORIENTED_EDGE ( 'NONE', *, *, #6354, .F. ) ;
#21173 = ORIENTED_EDGE ( 'NONE', *, *, #1788, .F. ) ;
#21174 = VERTEX_POINT ( 'NONE', #18674 ) ;
#21175 = CONTEXT_DEPENDENT_SHAPE_REPRESENTATION ( #18621, #7351 ) ;
#21176 = DIRECTION ( 'NONE',  ( 0.000000000000000000, -1.000000000000000000, 0.000000000000000000 ) ) ;
#21177 = CARTESIAN_POINT ( 'NONE',  ( 0.4803149606299212393, 0.000000000000000000, 0.2362204724409449064 ) ) ;
#21178 = ORIENTED_EDGE ( 'NONE', *, *, #25236, .F. ) ;
#21179 = CARTESIAN_POINT ( 'NONE',  ( 0.2223167940359795647, 0.2657206863494897542, 0.1377952755905510474 ) ) ;
#21180 = ORIENTED_EDGE ( 'NONE', *, *, #11293, .F. ) ;
#21181 = AXIS2_PLACEMENT_3D ( 'NONE', #4521, #17506, #26126 ) ;
#21182 = AXIS2_PLACEMENT_3D ( 'NONE', #6494, #15125, #23733 ) ;
#21183 = VERTEX_POINT ( 'NONE', #20810 ) ;
#21184 = CARTESIAN_POINT ( 'NONE',  ( -0.3215969074633125979, 0.3838795254899315390, 0.2574819596263889787 ) ) ;
#21185 = CIRCLE ( 'NONE', #3980, 0.5007874015748031704 ) ;
#21186 = AXIS2_PLACEMENT_3D ( 'NONE', #21340, #16960, #4105 ) ;
#21187 = DIRECTION ( 'NONE',  ( 0.9790454724845839563, -0.1018208755700887314, -0.1763589297585421989 ) ) ;
#21188 = DIRECTION ( 'NONE',  ( -1.000000000000000000, -1.000000000000000078E-15, 0.000000000000000000 ) ) ;
#21189 = CARTESIAN_POINT ( 'NONE',  ( -0.4354858238158328398, -0.8080706055940760635, -0.04854564796270125632 ) ) ;
#21190 = EDGE_CURVE ( 'NONE', #22807, #11452, #3712, .T. ) ;
#21191 = CARTESIAN_POINT ( 'NONE',  ( 0.4793172621399192090, 0.1288129352161812569, -1.569881889763779625 ) ) ;
#21192 = CARTESIAN_POINT ( 'NONE',  ( -0.08530183727034107433, 0.03937007874015742426, -0.06819097667594002654 ) ) ;
#21193 = B_SPLINE_CURVE_WITH_KNOTS ( 'NONE', 3,
 ( #27565, #2123, #14870, #10451, #184, #19070 ),
 .UNSPECIFIED., .F., .F.,
 ( 4, 2, 4 ),
 ( 0.3000437156586439613, 0.3015484798814579981, 0.3030532441042709801 ),
 .UNSPECIFIED. ) ;
#21194 = EDGE_CURVE ( 'NONE', #1637, #8715, #429, .T. ) ;
#21195 = PLANE ( 'NONE',  #18572 ) ;
#21196 = ORIENTED_EDGE ( 'NONE', *, *, #4096, .F. ) ;
#21197 = CARTESIAN_POINT ( 'NONE',  ( -0.1447526197146041249, -0.3977045540727763839, 0.06102165354330708891 ) ) ;
#21198 = EDGE_LOOP ( 'NONE', ( #25060, #13028, #11933, #5663, #10362 ) ) ;
#21199 = CARTESIAN_POINT ( 'NONE',  ( -0.03532354024591893848, -0.8267716535433071723, 0.000000000000000000 ) ) ;
#21200 = CARTESIAN_POINT ( 'NONE',  ( -0.4685039370078740717, 0.000000000000000000, -0.01377952755905511792 ) ) ;
#21201 = AXIS2_PLACEMENT_3D ( 'NONE', #27777, #27356, #2054 ) ;
#21202 = ORIENTED_EDGE ( 'NONE', *, *, #8676, .F. ) ;
#21203 = CONICAL_SURFACE ( 'NONE', #17583, 0.3039508883504944969, 0.2407725888118948110 ) ;
#21204 = CARTESIAN_POINT ( 'NONE',  ( 0.000000000000000000, 0.000000000000000000, 0.01181102362204724393 ) ) ;
#21205 = CARTESIAN_POINT ( 'NONE',  ( 0.3642352168757561071, 0.4152525734086270348, 0.9202755905511811330 ) ) ;
#21206 = VERTEX_POINT ( 'NONE', #23378 ) ;
#21207 = CARTESIAN_POINT ( 'NONE',  ( -0.3593781546376668135, 0.000000000000000000, -0.2755905511811023723 ) ) ;
#21208 = VERTEX_POINT ( 'NONE', #20953 ) ;
#21209 = FACE_OUTER_BOUND ( 'NONE', #10185, .T. ) ;
#21210 = CARTESIAN_POINT ( 'NONE',  ( -0.0006679551606482677165, 0.5322830454629158270, 0.3401574803149606252 ) ) ;
#21211 = DIRECTION ( 'NONE',  ( 1.000000000000000000, 0.000000000000000000, 0.000000000000000000 ) ) ;
#21212 = CARTESIAN_POINT ( 'NONE',  ( -0.5085287184740916455, -0.06690297524250585215, -1.550196850393700920 ) ) ;
#21213 = EDGE_CURVE ( 'NONE', #1342, #15191, #11708, .T. ) ;
#21214 = ADVANCED_FACE ( 'NONE', ( #6271 ), #23515, .F. ) ;
#21215 = CARTESIAN_POINT ( 'NONE',  ( -0.1968503937007874127, -0.4724409448818898127, 0.8182917201112815953 ) ) ;
#21216 = ORIENTED_EDGE ( 'NONE', *, *, #9385, .F. ) ;
#21217 = DIRECTION ( 'NONE',  ( 0.000000000000000000, 0.000000000000000000, 1.000000000000000000 ) ) ;
#21218 = CARTESIAN_POINT ( 'NONE',  ( 0.3239425792934409465, -0.08676778863010950471, 1.973425196850393970 ) ) ;
#21219 = FACE_OUTER_BOUND ( 'NONE', #17157, .T. ) ;
#21220 = AXIS2_PLACEMENT_3D ( 'NONE', #17810, #19807, #19681 ) ;
#21221 = CARTESIAN_POINT ( 'NONE',  ( 0.0005696707463077370576, 0.4606295689977898400, 0.1771653543307089018 ) ) ;
#21222 = VECTOR ( 'NONE', #15815, 39.37007874015748143 ) ;
#21223 = CARTESIAN_POINT ( 'NONE',  ( 0.2762247810519068980, 0.4783323773986306038, 0.9399606299212598381 ) ) ;
#21224 = CARTESIAN_POINT ( 'NONE',  ( 0.2423050875943940918, 0.2890362931940642088, 0.1992150590373740204 ) ) ;
#21225 = ADVANCED_FACE ( 'NONE', ( #3558 ), #12189, .T. ) ;
#21226 = FACE_OUTER_BOUND ( 'NONE', #8249, .T. ) ;
#21227 = EDGE_LOOP ( 'NONE', ( #8815, #15911 ) ) ;
#21228 = LINE ( 'NONE', #17264, #16433 ) ;
#21229 = CIRCLE ( 'NONE', #10857, 0.05216535433070866590 ) ;
#21230 = EDGE_LOOP ( 'NONE', ( #19462, #8494 ) ) ;
#21231 = VERTEX_POINT ( 'NONE', #12893 ) ;
#21232 = B_SPLINE_CURVE_WITH_KNOTS ( 'NONE', 3,
 ( #15135, #12988, #17509, #26128, #21618, #6783 ),
 .UNSPECIFIED., .F., .F.,
 ( 4, 2, 4 ),
 ( 0.000000000000000000, 0.2500000000000000000, 0.5000000000000000000 ),
 .UNSPECIFIED. ) ;
#21233 = CARTESIAN_POINT ( 'NONE',  ( -0.2564944395535840860, 0.4441657790094369895, -1.550196850393700920 ) ) ;
#21234 = CARTESIAN_POINT ( 'NONE',  ( -0.4954734376818675790, -0.2860009521627228657, 0.9399606299212597271 ) ) ;
#21235 = DIRECTION ( 'NONE',  ( 0.000000000000000000, -1.000000000000000000, 0.000000000000000000 ) ) ;
#21236 = DIRECTION ( 'NONE',  ( 0.000000000000000000, 1.000000000000000000, 0.000000000000000000 ) ) ;
#21237 = CARTESIAN_POINT ( 'NONE',  ( -0.4004922687717342167, -0.3511586785142652989, 1.747047244094487972 ) ) ;
#21238 = CARTESIAN_POINT ( 'NONE',  ( 0.000000000000000000, 0.000000000000000000, 0.1377952755905511584 ) ) ;
#21239 = ORIENTED_EDGE ( 'NONE', *, *, #24840, .F. ) ;
#21240 = CARTESIAN_POINT ( 'NONE',  ( -0.6002207073317223918, -0.5625436374629609881, -0.9710811323272637852 ) ) ;
#21241 = ADVANCED_FACE ( 'NONE', ( #17675 ), #15451, .F. ) ;
#21242 = CIRCLE ( 'NONE', #16730, 0.6995255587571318490 ) ;
#21243 = CARTESIAN_POINT ( 'NONE',  ( -0.08582064676143620618, 0.3030881253039517387, -3.222721154529648135 ) ) ;
#21244 = DIRECTION ( 'NONE',  ( 0.000000000000000000, 1.000000000000000000, 0.000000000000000000 ) ) ;
#21245 = DIRECTION ( 'NONE',  ( -0.000000000000000000, -1.000000000000000000, -0.000000000000000000 ) ) ;
#21246 = DIRECTION ( 'NONE',  ( 1.000000000000000000, 0.000000000000000000, 0.000000000000000000 ) ) ;
#21247 = ORIENTED_EDGE ( 'NONE', *, *, #209, .T. ) ;
#21248 = CARTESIAN_POINT ( 'NONE',  ( -1.466875984251968630E-17, 0.000000000000000000, -0.4566929133858267376 ) ) ;
#21249 = LINE ( 'NONE', #12344, #16826 ) ;
#21250 = ADVANCED_FACE ( 'NONE', ( #6961, #23652 ), #4818, .T. ) ;
#21251 = EDGE_LOOP ( 'NONE', ( #27057, #26189, #22057, #1291, #11731, #7896 ) ) ;
#21252 = ADVANCED_FACE ( 'NONE', ( #2160 ), #11323, .T. ) ;
#21253 = CARTESIAN_POINT ( 'NONE',  ( -0.2796934465393912106, 0.3645739570812651653, -1.928289503579152742 ) ) ;
#21254 = CARTESIAN_POINT ( 'NONE',  ( 0.4585215200179055817, -0.03001016326913584151, -1.928289503579156516 ) ) ;
#21255 = CARTESIAN_POINT ( 'NONE',  ( -0.3020979083623086536, 0.3591256245825952265, 0.07637795275590551769 ) ) ;
#21256 = EDGE_CURVE ( 'NONE', #10004, #25, #349, .T. ) ;
#21257 = CIRCLE ( 'NONE', #1403, 1.131889763779527547 ) ;
#21258 = VERTEX_POINT ( 'NONE', #8517 ) ;
#21259 = ORIENTED_EDGE ( 'NONE', *, *, #26321, .T. ) ;
#21260 = ORIENTED_EDGE ( 'NONE', *, *, #5680, .T. ) ;
#21261 = CARTESIAN_POINT ( 'NONE',  ( -0.4769977115679039370, -0.5686613684786834266, -0.07408240853524410141 ) ) ;
#21262 = CARTESIAN_POINT ( 'NONE',  ( 4.821444091131312140E-17, -1.707404996040164512E-16, 0.3937007874015748254 ) ) ;
#21263 = CARTESIAN_POINT ( 'NONE',  ( 0.2663596103035382745, -0.4612490782035122416, 1.747047244094488194 ) ) ;
#21264 = FACE_OUTER_BOUND ( 'NONE', #2205, .T. ) ;
#21265 = ORIENTED_EDGE ( 'NONE', *, *, #3506, .F. ) ;
#21266 = ( BOUNDED_CURVE ( )  B_SPLINE_CURVE ( 2, ( #24621, #17843, #2464 ),
 .UNSPECIFIED., .F., .T. ) 
 B_SPLINE_CURVE_WITH_KNOTS ( ( 3, 3 ),
 ( 0.000000000000000000, 0.5842180690389578990 ),
 .UNSPECIFIED. ) 
 CURVE ( )  GEOMETRIC_REPRESENTATION_ITEM ( )  RATIONAL_B_SPLINE_CURVE ( ( 1.000000000000000000, 1.154700538379249908, 1.000000000000000000 ) ) 
 REPRESENTATION_ITEM ( '' )  ) ;
#21267 = AXIS2_PLACEMENT_3D ( 'NONE', #7332, #3072, #5354 ) ;
#21268 = AXIS2_PLACEMENT_3D ( 'NONE', #10369, #8264, #16888 ) ;
#21269 = DIRECTION ( 'NONE',  ( 0.000000000000000000, 0.000000000000000000, 1.000000000000000000 ) ) ;
#21270 = CARTESIAN_POINT ( 'NONE',  ( -0.6098674607377709833, -0.5016125552355906736, 0.9930863283251144535 ) ) ;
#21271 = CARTESIAN_POINT ( 'NONE',  ( 0.1522836969735572310, 0.4941010236220472751, 0.000000000000000000 ) ) ;
#21272 = CARTESIAN_POINT ( 'NONE',  ( 0.05001895696127157259, -0.6334106509489122461, 0.07751973113670669602 ) ) ;
#21273 = VERTEX_POINT ( 'NONE', #17554 ) ;
#21274 = CARTESIAN_POINT ( 'NONE',  ( -0.3184841198566448206, 0.1570220809524502381, 1.953740157480315043 ) ) ;
#21275 = VERTEX_POINT ( 'NONE', #21658 ) ;
#21276 = CARTESIAN_POINT ( 'NONE',  ( -0.6259202480181347283, -0.06905013740392607069, -0.2391457790526826388 ) ) ;
#21277 = DIRECTION ( 'NONE',  ( 0.9930684569549264040, 0.05876869872891801738, -0.1017903720931950112 ) ) ;
#21278 = DIRECTION ( 'NONE',  ( 0.000000000000000000, 0.000000000000000000, -1.000000000000000000 ) ) ;
#21279 = ORIENTED_EDGE ( 'NONE', *, *, #26777, .T. ) ;
#21280 = DIRECTION ( 'NONE',  ( 0.000000000000000000, 0.000000000000000000, 1.000000000000000000 ) ) ;
#21281 = DIRECTION ( 'NONE',  ( 0.000000000000000000, -1.000000000000000000, 0.000000000000000000 ) ) ;
#21282 = EDGE_CURVE ( 'NONE', #15456, #26345, #9647, .T. ) ;
#21283 = VECTOR ( 'NONE', #17782, 39.37007874015748854 ) ;
#21284 = CARTESIAN_POINT ( 'NONE',  ( 0.1867299569291587802, -0.3233561589689049609, -3.115157480314960647 ) ) ;
#21285 = DIRECTION ( 'NONE',  ( 0.000000000000000000, 1.000000000000000000, 0.000000000000000000 ) ) ;
#21286 = DIRECTION ( 'NONE',  ( 1.000000000000000000, 0.000000000000000000, 0.000000000000000000 ) ) ;
#21287 = FACE_OUTER_BOUND ( 'NONE', #16889, .T. ) ;
#21288 = CYLINDRICAL_SURFACE ( 'NONE', #458, 0.2952755905264887182 ) ;
#21289 = EDGE_CURVE ( 'NONE', #9880, #19868, #15322, .T. ) ;
#21290 = ( GEOMETRIC_REPRESENTATION_CONTEXT ( 3 ) GLOBAL_UNCERTAINTY_ASSIGNED_CONTEXT ( ( #18622 ) ) GLOBAL_UNIT_ASSIGNED_CONTEXT ( ( #8487, #21488, #15555 ) ) REPRESENTATION_CONTEXT ( 'NONE', 'WORKASPACE' ) ) ;
#21291 = CARTESIAN_POINT ( 'NONE',  ( 0.4921259842519685179, -0.06441914069860961434, -1.569881889763779848 ) ) ;
#21292 = CARTESIAN_POINT ( 'NONE',  ( 0.000000000000000000, 0.000000000000000000, 0.1771653543307086520 ) ) ;
#21293 = EDGE_LOOP ( 'NONE', ( #6023, #25461, #10965, #16015 ) ) ;
#21294 = CARTESIAN_POINT ( 'NONE',  ( -0.5525004126151165096, 0.09742072959660473541, 0.07676968503937006694 ) ) ;
#21295 = ORIENTED_EDGE ( 'NONE', *, *, #7766, .T. ) ;
#21296 = CARTESIAN_POINT ( 'NONE',  ( -0.3480868068226445344, 0.1180291665653972477, -0.2426446119172513127 ) ) ;
#21297 = CARTESIAN_POINT ( 'NONE',  ( 0.09842519685039355370, 0.2165354330708661457, -3.548228346456693050 ) ) ;
#21298 = CARTESIAN_POINT ( 'NONE',  ( -0.4856708409200654608, 0.1649135259617025839, 1.766732283464566899 ) ) ;
#21299 = EDGE_CURVE ( 'NONE', #15651, #22705, #13432, .T. ) ;
#21300 = EDGE_LOOP ( 'NONE', ( #7608, #22296 ) ) ;
#21301 = AXIS2_PLACEMENT_3D ( 'NONE', #18678, #9935, #23232 ) ;
#21302 = VERTEX_POINT ( 'NONE', #25896 ) ;
#21303 = CARTESIAN_POINT ( 'NONE',  ( -0.2842490391651530390, -0.2180698645301770988, -3.115157480314960647 ) ) ;
#21304 = ORIENTED_EDGE ( 'NONE', *, *, #10132, .F. ) ;
#21305 = CARTESIAN_POINT ( 'NONE',  ( 0.4585215200179056372, -0.06002032661671170138, -1.928289503579156516 ) ) ;
#21306 = EDGE_LOOP ( 'NONE', ( #27297, #10109, #11870, #2188, #21239 ) ) ;
#21307 = ( NAMED_UNIT ( * ) PLANE_ANGLE_UNIT ( ) SI_UNIT ( $, .RADIAN. ) ) ;
#21308 = CARTESIAN_POINT ( 'NONE',  ( -0.3346456692913385988, 0.02190250779246044610, 1.973425196850393970 ) ) ;
#21309 = VERTEX_POINT ( 'NONE', #22059 ) ;
#21310 = ORIENTED_EDGE ( 'NONE', *, *, #27151, .F. ) ;
#21311 = AXIS2_PLACEMENT_3D ( 'NONE', #25093, #8156, #23132 ) ;
#21312 = CARTESIAN_POINT ( 'NONE',  ( 0.2180862235769585322, 0.4423390553432415273, -1.550196850393700920 ) ) ;
#21313 = DIRECTION ( 'NONE',  ( -0.2225209339563143096, 0.9749279121818237304, 0.000000000000000000 ) ) ;
#21314 = ORIENTED_EDGE ( 'NONE', *, *, #13011, .F. ) ;
#21315 = VERTEX_POINT ( 'NONE', #8789 ) ;
#21316 = DIRECTION ( 'NONE',  ( 1.000000000000000000, 0.000000000000000000, 0.000000000000000000 ) ) ;
#21317 = EDGE_CURVE ( 'NONE', #25524, #21624, #10358, .T. ) ;
#21318 = ITEM_DEFINED_TRANSFORMATION ( 'NONE', 'NONE', #336,  #11588 ) ;
#21319 = CARTESIAN_POINT ( 'NONE',  ( 0.000000000000000000, 0.000000000000000000, 0.02362204724409448786 ) ) ;
#21320 = CARTESIAN_POINT ( 'NONE',  ( -0.04992658653707177097, 0.3112137629952766438, -3.634044155725667302 ) ) ;
#21321 = DIRECTION ( 'NONE',  ( 1.000000000000000000, 0.000000000000000000, 0.000000000000000000 ) ) ;
#21322 = EDGE_LOOP ( 'NONE', ( #12299, #14558, #26087, #4693 ) ) ;
#21323 = PRODUCT_DEFINITION_SHAPE ( 'NONE', 'NONE',  #7589 ) ;
#21324 = ADVANCED_FACE ( 'NONE', ( #6409 ), #15341, .T. ) ;
#21325 = AXIS2_PLACEMENT_3D ( 'NONE', #14440, #16830, #20919 ) ;
#21326 = AXIS2_PLACEMENT_3D ( 'NONE', #19917, #15956, #3078 ) ;
#21327 = CARTESIAN_POINT ( 'NONE',  ( 0.000000000000000000, 0.000000000000000000, -0.1725236688546921415 ) ) ;
#21328 = DIRECTION ( 'NONE',  ( 0.000000000000000000, 0.000000000000000000, 1.000000000000000000 ) ) ;
#21329 = MANIFOLD_SOLID_BREP ( 'Deep Groove Ball Bearing 15x28x7', #25875 ) ;
#21330 = PLANE ( 'NONE',  #19115 ) ;
#21331 = CARTESIAN_POINT ( 'NONE',  ( -2.273123186440590970, -0.6468501409757874132, 2.145669291338582862 ) ) ;
#21332 = AXIS2_PLACEMENT_3D ( 'NONE', #14582, #1836, #1692 ) ;
#21333 = CARTESIAN_POINT ( 'NONE',  ( -0.4622328580205838366, -0.7042455557661343457, 0.02741266141520956948 ) ) ;
#21334 = CARTESIAN_POINT ( 'NONE',  ( -0.4620947063919693121, 0.08187111969648680487, 0.07637630773773071424 ) ) ;
#21335 = DIRECTION ( 'NONE',  ( 1.000000000000000000, 0.000000000000000000, 0.000000000000000000 ) ) ;
#21336 = CARTESIAN_POINT ( 'NONE',  ( 0.000000000000000000, 0.000000000000000000, -0.2342519685039370358 ) ) ;
#21337 = EDGE_CURVE ( 'NONE', #6451, #13218, #21171, .T. ) ;
#21338 = CARTESIAN_POINT ( 'NONE',  ( -0.03965503742771017692, 0.1968503937007873850, -3.203835717288081142 ) ) ;
#21339 = VERTEX_POINT ( 'NONE', #7651 ) ;
#21340 = CARTESIAN_POINT ( 'NONE',  ( 0.1259842519685039353, 0.000000000000000000, 0.000000000000000000 ) ) ;
#21341 = ORIENTED_EDGE ( 'NONE', *, *, #26746, .T. ) ;
#21342 = AXIS2_PLACEMENT_3D ( 'NONE', #15621, #24085, #6998 ) ;
#21343 = CARTESIAN_POINT ( 'NONE',  ( -0.5761865902011245044, 1.104160307813825792, -0.07772139087856803907 ) ) ;
#21344 = CARTESIAN_POINT ( 'NONE',  ( -0.1771653543307086520, 0.000000000000000000, 0.000000000000000000 ) ) ;
#21345 = CARTESIAN_POINT ( 'NONE',  ( 0.03607471876262465654, 0.5511811023622047445, 0.9202755905511811330 ) ) ;
#21346 = DIRECTION ( 'NONE',  ( 0.000000000000000000, 0.000000000000000000, 1.000000000000000000 ) ) ;
#21347 = ORIENTED_EDGE ( 'NONE', *, *, #15441, .T. ) ;
#21348 = DIRECTION ( 'NONE',  ( -0.000000000000000000, -1.000000000000000000, -0.000000000000000000 ) ) ;
#21349 = CONICAL_SURFACE ( 'NONE', #12742, 0.4537419570391968415, 1.365720138124999927 ) ;
#21350 = LINE ( 'NONE', #443, #6408 ) ;
#21351 = PLANE ( 'NONE',  #21766 ) ;
#21352 = DIRECTION ( 'NONE',  ( 1.000000000000000000, 0.000000000000000000, 0.000000000000000000 ) ) ;
#21353 = EDGE_CURVE ( 'NONE', #10570, #23745, #23451, .T. ) ;
#21354 = ORIENTED_EDGE ( 'NONE', *, *, #4808, .F. ) ;
#21355 = FACE_OUTER_BOUND ( 'NONE', #23104, .T. ) ;
#21356 = CARTESIAN_POINT ( 'NONE',  ( 0.2223167940359795092, 0.2657206863494898097, 0.1478915661212649724 ) ) ;
#21357 = VERTEX_POINT ( 'NONE', #22621 ) ;
#21358 = ORIENTED_EDGE ( 'NONE', *, *, #3152, .F. ) ;
#21359 = DIRECTION ( 'NONE',  ( 0.000000000000000000, 0.000000000000000000, -1.000000000000000000 ) ) ;
#21360 = AXIS2_PLACEMENT_3D ( 'NONE', #3312, #9685, #22833 ) ;
#21361 = DIRECTION ( 'NONE',  ( 0.000000000000000000, -1.000000000000000000, 0.000000000000000000 ) ) ;
#21362 = AXIS2_PLACEMENT_3D ( 'NONE', #2167, #8795, #26172 ) ;
#21363 = CARTESIAN_POINT ( 'NONE',  ( 0.4783323773986625782, 0.2762247810518427271, 0.9399606299212598381 ) ) ;
#21364 = CARTESIAN_POINT ( 'NONE',  ( -0.8725268807032540153, 0.000000000000000000, -1.052618110236220428 ) ) ;
#21365 = VERTEX_POINT ( 'NONE', #5533 ) ;
#21366 = CARTESIAN_POINT ( 'NONE',  ( -0.04673614183172691838, 0.3552064049866300866, -3.115157480314961091 ) ) ;
#21367 = AXIS2_PLACEMENT_3D ( 'NONE', #22434, #26809, #7456 ) ;
#21368 = CIRCLE ( 'NONE', #11406, 0.4267795243146149664 ) ;
#21369 = MANIFOLD_SOLID_BREP ( 'Output Shaft', #4240 ) ;
#21370 = CIRCLE ( 'NONE', #9163, 0.4803149606299212393 ) ;
#21371 = APPLICATION_CONTEXT ( 'automotive_design' ) ;
#21372 = ORIENTED_EDGE ( 'NONE', *, *, #14581, .T. ) ;
#21373 = CARTESIAN_POINT ( 'NONE',  ( -0.3382184156749268311, 0.3855916753034290823, -1.550196850393700920 ) ) ;
#21374 = CARTESIAN_POINT ( 'NONE',  ( -6.132876883919029269E-17, -0.5007874015748031704, 0.09685039370078740717 ) ) ;
#21375 = CARTESIAN_POINT ( 'NONE',  ( 0.03008364706454716778, -0.2273032555864669124, 2.185478346456692557E-17 ) ) ;
#21376 = DIRECTION ( 'NONE',  ( -1.000000000000000000, 0.000000000000000000, 0.000000000000000000 ) ) ;
#21377 = CARTESIAN_POINT ( 'NONE',  ( -0.1327957795767781002, 0.4954247181592900118, -1.550196850393701364 ) ) ;
#21378 = CIRCLE ( 'NONE', #9612, 0.3771653543307086909 ) ;
#21379 = CARTESIAN_POINT ( 'NONE',  ( -0.0007683673430022958887, 0.7042519390035199001, 0.3281099440177754345 ) ) ;
#21380 = ORIENTED_EDGE ( 'NONE', *, *, #22453, .F. ) ;
#21381 = CARTESIAN_POINT ( 'NONE',  ( 0.000000000000000000, 0.000000000000000000, 0.2362204724409449064 ) ) ;
#21382 = EDGE_CURVE ( 'NONE', #4526, #21365, #22480, .T. ) ;
#21383 = CARTESIAN_POINT ( 'NONE',  ( 0.6791338582677166613, 0.000000000000000000, 0.000000000000000000 ) ) ;
#21384 = CARTESIAN_POINT ( 'NONE',  ( 1.197070535079588716, 0.07874015748031495954, -1.315180771300060503 ) ) ;
#21385 = DIRECTION ( 'NONE',  ( 0.000000000000000000, 0.000000000000000000, 1.000000000000000000 ) ) ;
#21386 = EDGE_LOOP ( 'NONE', ( #7796, #22664 ) ) ;
#21387 = SURFACE_STYLE_USAGE ( .BOTH. , #20817 ) ;
#21388 = AXIS2_PLACEMENT_3D ( 'NONE', #17222, #8742, #23994 ) ;
#21389 = CARTESIAN_POINT ( 'NONE',  ( -0.06894484415258525511, -0.05111597790624471116, -0.4724409448841456749 ) ) ;
#21390 = CIRCLE ( 'NONE', #2436, 0.3031496062992122820 ) ;
#21391 = VERTEX_POINT ( 'NONE', #11462 ) ;
#21392 = CARTESIAN_POINT ( 'NONE',  ( -0.4763861460130593972, 0.1275996891957734969, -1.550196850393700920 ) ) ;
#21393 = CARTESIAN_POINT ( 'NONE',  ( 0.4498374011143674855, 0.05926487674658936083, -1.934055118110236338 ) ) ;
#21394 = AXIS2_PLACEMENT_3D ( 'NONE', #2002, #25881, #21644 ) ;
#21395 = CARTESIAN_POINT ( 'NONE',  ( 0.000000000000000000, 0.8661417322803149910, -0.3937007874015748254 ) ) ;
#21396 = EDGE_CURVE ( 'NONE', #13772, #2222, #8539, .T. ) ;
#21397 = ORIENTED_EDGE ( 'NONE', *, *, #23182, .F. ) ;
#21398 = CARTESIAN_POINT ( 'NONE',  ( -0.5172021183779732523, -0.3148976862790665576, -0.2992753242159311156 ) ) ;
#21399 = CARTESIAN_POINT ( 'NONE',  ( 0.3346456692913385988, 4.098227477461614641E-17, 2.426181102355854158 ) ) ;
#21400 = CARTESIAN_POINT ( 'NONE',  ( 0.5144970376935932288, -0.1378076643338853879, 1.747047244094488194 ) ) ;
#21401 = DIRECTION ( 'NONE',  ( 0.000000000000000000, 0.000000000000000000, -1.000000000000000000 ) ) ;
#21402 = ADVANCED_FACE ( 'NONE', ( #9760 ), #20079, .F. ) ;
#21403 = AXIS2_PLACEMENT_3D ( 'NONE', #14536, #23429, #1792 ) ;
#21404 = CARTESIAN_POINT ( 'NONE',  ( -4.821283464566928349E-18, 0.000000000000000000, -0.3779527559055118058 ) ) ;
#21405 = AXIS2_PLACEMENT_3D ( 'NONE', #2767, #15785, #26372 ) ;
#21406 = CARTESIAN_POINT ( 'NONE',  ( 0.6889763779527560139, 8.437527159479796553E-17, -0.1377952755905511861 ) ) ;
#21407 = CARTESIAN_POINT ( 'NONE',  ( 0.1431838228103888555, 0.4219236230596360993, -1.934055118110237004 ) ) ;
#21408 = EDGE_CURVE ( 'NONE', #2747, #21183, #6967, .T. ) ;
#21409 = VERTEX_POINT ( 'NONE', #24442 ) ;
#21410 = CARTESIAN_POINT ( 'NONE',  ( -0.2669480828848092013, 0.2341512108694271399, 1.953740157480315043 ) ) ;
#21411 = ORIENTED_EDGE ( 'NONE', *, *, #10267, .T. ) ;
#21412 = CARTESIAN_POINT ( 'NONE',  ( -0.5513845672049195734, -0.2358478765533125465, -0.2710066445262201973 ) ) ;
#21413 = DIRECTION ( 'NONE',  ( -1.000000000000000000, 0.000000000000000000, 0.000000000000000000 ) ) ;
#21414 = CARTESIAN_POINT ( 'NONE',  ( -0.1480156394741835579, -0.5526079293737254927, 0.9399606299212598381 ) ) ;
#21415 = EDGE_CURVE ( 'NONE', #13221, #11845, #8325, .T. ) ;
#21416 = MANIFOLD_SOLID_BREP ( 'Bearing Cone', #13694 ) ;
#21417 = B_SPLINE_CURVE_WITH_KNOTS ( 'NONE', 3,
 ( #17245, #4531, #13135, #21765, #7472, #986 ),
 .UNSPECIFIED., .F., .F.,
 ( 4, 2, 4 ),
 ( 0.000000000000000000, 0.2500000000000000000, 0.5000000000000000000 ),
 .UNSPECIFIED. ) ;
#21418 = CARTESIAN_POINT ( 'NONE',  ( 0.2249706821157846648, -0.6026734741281122298, -0.4922986699466661009 ) ) ;
#21419 = CARTESIAN_POINT ( 'NONE',  ( 0.000000000000000000, 0.000000000000000000, 0.2362204724409449064 ) ) ;
#21420 = CARTESIAN_POINT ( 'NONE',  ( -0.1968503937007874127, 0.07874015748031495954, 0.04546065111729331171 ) ) ;
#21421 = AXIS2_PLACEMENT_3D ( 'NONE', #6772, #303, #26116 ) ;
#21422 = CARTESIAN_POINT ( 'NONE',  ( 0.1651192144506304360, -0.3349073414798397486, -3.115157480314960647 ) ) ;
#21423 = DIRECTION ( 'NONE',  ( 0.000000000000000000, -1.000000000000000000, 0.000000000000000000 ) ) ;
#21424 = CYLINDRICAL_SURFACE ( 'NONE', #8021, 0.8267716535433071723 ) ;
#21425 = DIRECTION ( 'NONE',  ( -1.000000000000000000, 0.000000000000000000, 0.000000000000000000 ) ) ;
#21426 = CARTESIAN_POINT ( 'NONE',  ( 0.000000000000000000, 0.3937007874015748254, 0.2362204724409449064 ) ) ;
#21427 = CARTESIAN_POINT ( 'NONE',  ( 0.3024344094364739832, -0.3935368318888683437, -1.569881889763779625 ) ) ;
#21428 = CARTESIAN_POINT ( 'NONE',  ( -0.7171569026236448430, -0.1628805401839451827, 0.1960773254322785986 ) ) ;
#21429 = VECTOR ( 'NONE', #2329, 39.37007874015748143 ) ;
#21430 = ORIENTED_EDGE ( 'NONE', *, *, #1826, .F. ) ;
#21431 = CARTESIAN_POINT ( 'NONE',  ( 0.5377323685532543474, 0.4294741335735771659, 0.1322818203437346463 ) ) ;
#21432 = ORIENTED_EDGE ( 'NONE', *, *, #14714, .F. ) ;
#21433 = DIRECTION ( 'NONE',  ( 1.000000000000000000, 0.000000000000000000, 0.000000000000000000 ) ) ;
#21434 = CARTESIAN_POINT ( 'NONE',  ( 0.3512268162760113777, -0.4004221243553278131, 1.747047244094488194 ) ) ;
#21435 = SHAPE_DEFINITION_REPRESENTATION ( #24888, #24703 ) ;
#21436 = CARTESIAN_POINT ( 'NONE',  ( -0.3382184156732009339, -0.3855916753051547574, 1.766732283464566899 ) ) ;
#21437 = CARTESIAN_POINT ( 'NONE',  ( -0.4441657790107820802, -0.2564944395515947884, 1.747047244094488194 ) ) ;
#21438 = AXIS2_PLACEMENT_3D ( 'NONE', #8031, #16358, #3336 ) ;
#21439 = DIRECTION ( 'NONE',  ( 1.000000000000000000, 0.000000000000000000, 0.000000000000000000 ) ) ;
#21440 = VERTEX_POINT ( 'NONE', #14447 ) ;
#21441 = EDGE_CURVE ( 'NONE', #14551, #11993, #27435, .T. ) ;
#21442 = EDGE_LOOP ( 'NONE', ( #6071, #2097 ) ) ;
#21444 = CARTESIAN_POINT ( 'NONE',  ( -0.3535721684717625934, 0.1200583359873131500, -3.115157480314960647 ) ) ;
#21443 = CARTESIAN_POINT ( 'NONE',  ( -0.1968503937007874127, -5.733057234251967840E-18, -0.1476377952755905387 ) ) ;
#21445 = EDGE_LOOP ( 'NONE', ( #20123, #5519, #22114, #12709, #20598 ) ) ;
#21446 = VERTEX_POINT ( 'NONE', #16691 ) ;
#21447 = CARTESIAN_POINT ( 'NONE',  ( -0.1632039128461710842, -0.4501088385475445208, 0.08349695147787532246 ) ) ;
#21448 = VERTEX_POINT ( 'NONE', #22910 ) ;
#21449 = CARTESIAN_POINT ( 'NONE',  ( 0.3339160553493882300, 0.7695422168913326200, -0.7725620623222638761 ) ) ;
#21450 = EDGE_CURVE ( 'NONE', #25692, #14534, #12987, .T. ) ;
#21451 = CARTESIAN_POINT ( 'NONE',  ( -0.3239425792934402248, -0.08676778863011362641, 1.973425196850393970 ) ) ;
#21452 = ORIENTED_EDGE ( 'NONE', *, *, #6493, .F. ) ;
#21453 = EDGE_LOOP ( 'NONE', ( #26779, #8727, #10603, #15678, #9187, #19677 ) ) ;
#21454 = AXIS2_PLACEMENT_3D ( 'NONE', #17917, #13149, #21502 ) ;
#21455 = CARTESIAN_POINT ( 'NONE',  ( 0.06441834428466734763, 0.4889536969035060965, -1.550196850393700920 ) ) ;
#21456 = DIRECTION ( 'NONE',  ( 1.000000000000000000, 0.000000000000000000, 0.000000000000000000 ) ) ;
#21457 = AXIS2_PLACEMENT_3D ( 'NONE', #12595, #27860, #21217 ) ;
#21458 = EDGE_LOOP ( 'NONE', ( #6813, #1711 ) ) ;
#21459 = EDGE_LOOP ( 'NONE', ( #11842, #23064, #6249, #20780 ) ) ;
#21460 = ORIENTED_EDGE ( 'NONE', *, *, #16074, .F. ) ;
#21461 = CARTESIAN_POINT ( 'NONE',  ( -0.03794311743615354227, 0.6358669483114146592, -0.5146366652944387443 ) ) ;
#21462 = DIRECTION ( 'NONE',  ( 1.000000000000000000, 0.000000000000000000, 0.000000000000000000 ) ) ;
#21463 = DIRECTION ( 'NONE',  ( 0.000000000000000000, -1.000000000000000000, 0.000000000000000000 ) ) ;
#21464 = CARTESIAN_POINT ( 'NONE',  ( 0.4620608682196457040, 0.08206165078054626638, 0.07637795275590551769 ) ) ;
#21465 = CIRCLE ( 'NONE', #7013, 0.7500000000000001110 ) ;
#21466 = EDGE_CURVE ( 'NONE', #11023, #25542, #5497, .T. ) ;
#21467 = CARTESIAN_POINT ( 'NONE',  ( -0.07874015748031495954, -0.02322071673952561324, -0.4680922445168273494 ) ) ;
#21468 = DIRECTION ( 'NONE',  ( -1.000000000000000000, 0.000000000000000000, 0.000000000000000000 ) ) ;
#21469 = CARTESIAN_POINT ( 'NONE',  ( -0.06181127634704723650, -1.564461769117756029, 2.027559055118110187 ) ) ;
#21470 = CARTESIAN_POINT ( 'NONE',  ( 0.2309201403895324856, 0.4006498629591504490, -1.928289503579156516 ) ) ;
#21471 = AXIS2_PLACEMENT_3D ( 'NONE', #7198, #22310, #13837 ) ;
#21472 = CARTESIAN_POINT ( 'NONE',  ( 0.3680051700917442714, -0.4526932812344531265, 5.543894897734252589E-17 ) ) ;
#21473 = CARTESIAN_POINT ( 'NONE',  ( -0.3334645669291338987, 0.8151331854455394765, -1.007197927683596506 ) ) ;
#21474 = EDGE_CURVE ( 'NONE', #27620, #10277, #12262, .T. ) ;
#21475 = AXIS2_PLACEMENT_3D ( 'NONE', #24819, #1375, #14091 ) ;
#21476 = CARTESIAN_POINT ( 'NONE',  ( 0.1516263115863346334, 0.2937912646890007973, 0.3972688187320929099 ) ) ;
#21477 = ORIENTED_EDGE ( 'NONE', *, *, #27294, .T. ) ;
#21478 = CARTESIAN_POINT ( 'NONE',  ( -2.685748425196850164E-17, 0.000000000000000000, -3.745078740157480546 ) ) ;
#21479 = EDGE_CURVE ( 'NONE', #24310, #3886, #9270, .T. ) ;
#21480 = AXIS2_PLACEMENT_3D ( 'NONE', #24071, #4707, #2583 ) ;
#21481 = ORIENTED_EDGE ( 'NONE', *, *, #5527, .F. ) ;
#21482 = DIRECTION ( 'NONE',  ( 0.000000000000000000, 1.000000000000000000, 0.000000000000000000 ) ) ;
#21483 = DIRECTION ( 'NONE',  ( 0.8571673003991031603, 0.000000000000000000, 0.5150380754143460971 ) ) ;
#21484 = CARTESIAN_POINT ( 'NONE',  ( -0.5511811023622048555, 0.000000000000000000, 0.9399606299212598381 ) ) ;
#21485 = DIRECTION ( 'NONE',  ( 0.7818314824680303587, 0.6234898018587330393, -0.000000000000000000 ) ) ;
#21486 = VERTEX_POINT ( 'NONE', #6108 ) ;
#21487 = CARTESIAN_POINT ( 'NONE',  ( 0.3002886982018043160, -0.1727973894384573772, 0.1276989850532580795 ) ) ;
#21488 = ( NAMED_UNIT ( * ) PLANE_ANGLE_UNIT ( ) SI_UNIT ( $, .RADIAN. ) ) ;
#21489 = AXIS2_PLACEMENT_3D ( 'NONE', #23046, #9752, #8071 ) ;
#21490 = FACE_OUTER_BOUND ( 'NONE', #8507, .T. ) ;
#21491 = DIRECTION ( 'NONE',  ( 0.000000000000000000, 0.000000000000000000, 1.000000000000000000 ) ) ;
#21492 = CARTESIAN_POINT ( 'NONE',  ( -0.5099673189325635292, -0.1157175986330993001, 0.1392975274259370122 ) ) ;
#21493 = EDGE_CURVE ( 'NONE', #3818, #15551, #22624, .T. ) ;
#21494 = AXIS2_PLACEMENT_3D ( 'NONE', #7817, #16997, #10195 ) ;
#21495 = ORIENTED_EDGE ( 'NONE', *, *, #2298, .F. ) ;
#21496 = DIRECTION ( 'NONE',  ( -0.9396926207859082059, -0.3420201433256691015, 0.000000000000000000 ) ) ;
#21497 = CARTESIAN_POINT ( 'NONE',  ( -0.09842519685039366473, 0.1968503937007873850, -3.272637795275590733 ) ) ;
#21498 = DIRECTION ( 'NONE',  ( 0.000000000000000000, 0.000000000000000000, -1.000000000000000000 ) ) ;
#21499 = DIRECTION ( 'NONE',  ( 0.000000000000000000, 0.000000000000000000, -1.000000000000000000 ) ) ;
#21500 = LINE ( 'NONE', #4126, #1170 ) ;
#21501 = DIRECTION ( 'NONE',  ( -1.000000000000000000, 0.000000000000000000, 0.000000000000000000 ) ) ;
#21502 = DIRECTION ( 'NONE',  ( 0.000000000000000000, 0.000000000000000000, -1.000000000000000000 ) ) ;
#21503 = CARTESIAN_POINT ( 'NONE',  ( -0.2860899518037490763, 0.4954156765914824456, 0.9399606299212598381 ) ) ;
#21504 = FACE_OUTER_BOUND ( 'NONE', #5498, .T. ) ;
#21505 = ORIENTED_EDGE ( 'NONE', *, *, #7082, .T. ) ;
#21506 = CARTESIAN_POINT ( 'NONE',  ( 0.1525037638700916243, -0.2637554987713725541, 0.4194810972668290283 ) ) ;
#21507 = EDGE_CURVE ( 'NONE', #16084, #26083, #12588, .T. ) ;
#21508 = CARTESIAN_POINT ( 'NONE',  ( -0.4527559054764770385, -0.02963280468031422032, -1.934055118110236338 ) ) ;
#21509 = ORIENTED_EDGE ( 'NONE', *, *, #9563, .F. ) ;
#21510 = AXIS2_PLACEMENT_3D ( 'NONE', #8486, #17108, #23085 ) ;
#21511 = ADVANCED_FACE ( 'NONE', ( #16533, #21209 ), #27713, .T. ) ;
#21512 = ORIENTED_EDGE ( 'NONE', *, *, #14788, .F. ) ;
#21513 = CIRCLE ( 'NONE', #9298, 1.092519685039370136 ) ;
#21514 = EDGE_CURVE ( 'NONE', #22691, #8098, #25587, .T. ) ;
#21515 = CARTESIAN_POINT ( 'NONE',  ( 0.4069448477569521661, 0.3121994997578569353, -1.550196850393700920 ) ) ;
#21516 = CARTESIAN_POINT ( 'NONE',  ( 0.6202606299212598540, -6.779653543307085645E-20, 0.000000000000000000 ) ) ;
#21517 = FACE_OUTER_BOUND ( 'NONE', #16285, .T. ) ;
#21518 = CARTESIAN_POINT ( 'NONE',  ( 0.5314960629921261503, -0.03489125111630842629, 1.747047244094488416 ) ) ;
#21519 = ORIENTED_EDGE ( 'NONE', *, *, #6214, .F. ) ;
#21520 = ORIENTED_EDGE ( 'NONE', *, *, #24031, .F. ) ;
#21521 = DIRECTION ( 'NONE',  ( 1.000000000000000000, 0.000000000000000000, 0.000000000000000000 ) ) ;
#21522 = CARTESIAN_POINT ( 'NONE',  ( 0.7171569026264477120, -0.1628805401845836165, 0.2763636194414290093 ) ) ;
#21523 = CARTESIAN_POINT ( 'NONE',  ( 0.6055690743987126590, 0.2581485381169799642, -0.4471263839182408883 ) ) ;
#21524 = ORIENTED_EDGE ( 'NONE', *, *, #22466, .F. ) ;
#21525 = DIRECTION ( 'NONE',  ( 0.000000000000000000, 0.000000000000000000, -1.000000000000000000 ) ) ;
#21526 = CARTESIAN_POINT ( 'NONE',  ( 0.000000000000000000, 0.000000000000000000, 2.090519358671640647E-11 ) ) ;
#21527 = CARTESIAN_POINT ( 'NONE',  ( 0.1120675189988346587, -0.7410715175625038897, 0.001857066358701141805 ) ) ;
#21528 = ORIENTED_EDGE ( 'NONE', *, *, #21983, .F. ) ;
#21529 = CARTESIAN_POINT ( 'NONE',  ( -0.4143458349576718547, -0.2398979215369355655, 0.1920935997051132493 ) ) ;
#21530 = CARTESIAN_POINT ( 'NONE',  ( -0.1275996891957733581, -0.4763861460130334735, -1.569881889763779625 ) ) ;
#21531 = CARTESIAN_POINT ( 'NONE',  ( 0.02963280468032102044, 0.4527559054764770385, -1.934055118110236338 ) ) ;
#21532 = B_SPLINE_CURVE_WITH_KNOTS ( 'NONE', 3,
 ( #6816, #23781, #4422, #23510, #23918, #2011 ),
 .UNSPECIFIED., .F., .F.,
 ( 4, 2, 4 ),
 ( 0.000000000000000000, 0.2500000000000000000, 0.5000000000000000000 ),
 .UNSPECIFIED. ) ;
#21533 = CARTESIAN_POINT ( 'NONE',  ( -8.632637795275590524E-16, -0.8267716535433071723, 0.000000000000000000 ) ) ;
#21534 = CARTESIAN_POINT ( 'NONE',  ( 0.1643029338967702813, -0.4497088275954951309, 0.1920935997051998190 ) ) ;
#21535 = CARTESIAN_POINT ( 'NONE',  ( -0.5632721120450597807, -0.2490672660460055143, -0.1109894576568373897 ) ) ;
#21536 = B_SPLINE_CURVE_WITH_KNOTS ( 'NONE', 3,
 ( #1008, #14289, #24720, #3668, #16683, #25292 ),
 .UNSPECIFIED., .F., .F.,
 ( 4, 2, 4 ),
 ( 0.3000437156586439613, 0.3015484798814569989, 0.3030532441042709801 ),
 .UNSPECIFIED. ) ;
#21537 = ( CONVERSION_BASED_UNIT ( 'INCH', #4306 ) LENGTH_UNIT ( ) NAMED_UNIT ( #12296 ) ) ;
#21538 = CARTESIAN_POINT ( 'NONE',  ( -0.09842519685039370636, 0.2165354330708661457, -3.272637795275590733 ) ) ;
#21539 = DIRECTION ( 'NONE',  ( 0.000000000000000000, 1.000000000000000000, 0.000000000000000000 ) ) ;
#21540 = CARTESIAN_POINT ( 'NONE',  ( -0.3362580771780888655, -0.1141156591734552583, 1.953740157480314599 ) ) ;
#21541 = DIRECTION ( 'NONE',  ( 1.000000000000000000, 0.000000000000000000, 0.000000000000000000 ) ) ;
#21542 = CIRCLE ( 'NONE', #26053, 0.1308464566929133932 ) ;
#21543 = CARTESIAN_POINT ( 'NONE',  ( 0.2937477835497820378, 0.3350125228554541312, -1.934055118110236560 ) ) ;
#21544 = CARTESIAN_POINT ( 'NONE',  ( -0.6722178168900768691, 0.03697663028270673641, -0.2369544657523791342 ) ) ;
#21545 = ORIENTED_EDGE ( 'NONE', *, *, #2149, .T. ) ;
#21546 = CARTESIAN_POINT ( 'NONE',  ( -0.3929158813954827245, 0.2268989272876178465, -1.934055118110236338 ) ) ;
#21547 = FACE_OUTER_BOUND ( 'NONE', #15172, .T. ) ;
#21548 = CARTESIAN_POINT ( 'NONE',  ( 0.1520645003235147619, -0.1970746732862649619, 0.4530975571996339046 ) ) ;
#21549 = CYLINDRICAL_SURFACE ( 'NONE', #18985, 0.1082677165354330312 ) ;
#21550 = DIRECTION ( 'NONE',  ( -1.000000000000000000, 0.000000000000000000, 0.000000000000000000 ) ) ;
#21551 = CARTESIAN_POINT ( 'NONE',  ( 0.2272836761397793726, 0.2962590301041582164, -3.115157480314960647 ) ) ;
#21552 = CARTESIAN_POINT ( 'NONE',  ( 0.3543307086614173040, -0.09842519685039370636, 1.205361022782828035E-17 ) ) ;
#21553 = SURFACE_STYLE_USAGE ( .BOTH. , #384 ) ;
#21554 = CARTESIAN_POINT ( 'NONE',  ( 0.000000000000000000, -4.081314960629921056E-17, -0.1692378991623492424 ) ) ;
#21555 = DIRECTION ( 'NONE',  ( 0.000000000000000000, 1.000000000000000000, 0.000000000000000000 ) ) ;
#21556 = ADVANCED_FACE ( 'NONE', ( #12997 ), #130, .F. ) ;
#21557 = AXIS2_PLACEMENT_3D ( 'NONE', #24443, #24589, #1017 ) ;
#21558 = EDGE_CURVE ( 'NONE', #10762, #11214, #15424, .T. ) ;
#21559 = CARTESIAN_POINT ( 'NONE',  ( 0.0005789221761808661720, 0.4692909815006409691, 0.1992125984251968684 ) ) ;
#21560 = ADVANCED_FACE ( 'NONE', ( #24862 ), #24716, .F. ) ;
#21561 = PRODUCT_RELATED_PRODUCT_CATEGORY ( 'part', '', ( #22884 ) ) ;
#21562 = EDGE_CURVE ( 'NONE', #5769, #24896, #9080, .T. ) ;
#21563 = ORIENTED_EDGE ( 'NONE', *, *, #7398, .F. ) ;
#21564 = CARTESIAN_POINT ( 'NONE',  ( 0.2720459371704843088, 0.3242117229735830830, 0.1377952755905511861 ) ) ;
#21565 = ORIENTED_EDGE ( 'NONE', *, *, #8978, .F. ) ;
#21566 = VERTEX_POINT ( 'NONE', #24014 ) ;
#21567 = VECTOR ( 'NONE', #18060, 39.37007874015748143 ) ;
#21568 = EDGE_CURVE ( 'NONE', #26519, #17531, #21350, .T. ) ;
#21569 = ADVANCED_FACE ( 'NONE', ( #19775 ), #25727, .T. ) ;
#21570 = CARTESIAN_POINT ( 'NONE',  ( 3.168943700787402105E-16, -0.07677165354330710290, 0.000000000000000000 ) ) ;
#21571 = CARTESIAN_POINT ( 'NONE',  ( 0.5118110236220471121, 0.06699590632655406941, 1.766732283464567121 ) ) ;
#21572 = LINE ( 'NONE', #2208, #16011 ) ;
#21573 = CARTESIAN_POINT ( 'NONE',  ( 0.06699507805370044644, -0.5085118447801416641, 1.766732283464566899 ) ) ;
#21574 = CARTESIAN_POINT ( 'NONE',  ( -0.3121994997598253052, -0.4069448477556119048, 1.747047244094488194 ) ) ;
#21575 = FILL_AREA_STYLE_COLOUR ( '', #23537 ) ;
#21576 = ORIENTED_EDGE ( 'NONE', *, *, #1280, .F. ) ;
#21577 = EDGE_LOOP ( 'NONE', ( #13099, #16558, #15109, #19904 ) ) ;
#21578 = VERTEX_POINT ( 'NONE', #4390 ) ;
#21579 = CARTESIAN_POINT ( 'NONE',  ( -0.2693339498142344746, -0.2362439534887506021, -3.115157480314960647 ) ) ;
#21580 = ORIENTED_EDGE ( 'NONE', *, *, #19588, .T. ) ;
#21581 = CARTESIAN_POINT ( 'NONE',  ( -0.5378903297326614874, 0.4292762795476984805, 0.3401599409343964431 ) ) ;
#21582 = SHAPE_REPRESENTATION_RELATIONSHIP ( 'NONE' , 'NONE' ,  #15008, #16079 ) ;
#21583 = VECTOR ( 'NONE', #5792, 39.37007874015748854 ) ;
#21584 = CARTESIAN_POINT ( 'NONE',  ( -0.02190250779246035590, 0.3346456692913385988, 1.953740157480315043 ) ) ;
#21585 = VERTEX_POINT ( 'NONE', #2260 ) ;
#21586 = EDGE_LOOP ( 'NONE', ( #11513, #17738, #392, #26523 ) ) ;
#21587 = CIRCLE ( 'NONE', #13003, 0.09842519685039370636 ) ;
#21588 = CARTESIAN_POINT ( 'NONE',  ( -1.928577543407793639E-16, 0.07874015748031491790, 1.811023622047243542 ) ) ;
#21589 = VECTOR ( 'NONE', #22879, 39.37007874015748854 ) ;
#21590 = EDGE_LOOP ( 'NONE', ( #7425, #15860 ) ) ;
#21591 = EDGE_LOOP ( 'NONE', ( #432, #23578, #6620, #27778 ) ) ;
#21592 = ORIENTED_EDGE ( 'NONE', *, *, #15719, .T. ) ;
#21593 = DIRECTION ( 'NONE',  ( -1.000000000000000000, 0.000000000000000000, 0.000000000000000000 ) ) ;
#21594 = CARTESIAN_POINT ( 'NONE',  ( 0.5905511811023621549, -0.3346456692913385988, 4.098227477461615257E-17 ) ) ;
#21595 = CARTESIAN_POINT ( 'NONE',  ( 0.3020979083623086536, 0.3591256245825952265, 0.1992125984251968684 ) ) ;
#21596 = AXIS2_PLACEMENT_3D ( 'NONE', #17132, #9054, #25753 ) ;
#21597 = CARTESIAN_POINT ( 'NONE',  ( -2.685748425196850164E-17, 0.000000000000000000, -3.745078740157480546 ) ) ;
#21598 = EDGE_LOOP ( 'NONE', ( #20632, #14130 ) ) ;
#21599 = CARTESIAN_POINT ( 'NONE',  ( -0.5043865966253989752, 0.1711654736997713921, 1.747047244094488416 ) ) ;
#21600 = CARTESIAN_POINT ( 'NONE',  ( -0.07874015748031495954, -0.01181091161850882261, -0.4653543306978102367 ) ) ;
#21601 = CONTEXT_DEPENDENT_SHAPE_REPRESENTATION ( #9628, #2587 ) ;
#21602 = MANIFOLD_SOLID_BREP ( 'O-Ring 36.5x2.65', #16405 ) ;
#21603 = EDGE_CURVE ( 'NONE', #24639, #764, #12998, .T. ) ;
#21604 = ADVANCED_FACE ( 'NONE', ( #21903 ), #1426, .T. ) ;
#21605 = CIRCLE ( 'NONE', #26093, 0.02362204724409448092 ) ;
#21606 = CARTESIAN_POINT ( 'NONE',  ( -0.5616721359164329463, 1.121275077793840946, 0.01914631898357971665 ) ) ;
#21607 = AXIS2_PLACEMENT_3D ( 'NONE', #10183, #13992, #5373 ) ;
#21608 = CARTESIAN_POINT ( 'NONE',  ( -0.2817828961649163078, 0.3666644560843324019, -1.928289503579156294 ) ) ;
#21609 = EDGE_CURVE ( 'NONE', #10683, #25047, #15861, .T. ) ;
#21610 = TOROIDAL_SURFACE ( 'NONE', #1315, 0.5610236220472440971, 0.1003937007874015908 ) ;
#21611 = DIRECTION ( 'NONE',  ( -1.000000000000000000, 0.000000000000000000, 0.000000000000000000 ) ) ;
#21612 = CARTESIAN_POINT ( 'NONE',  ( 0.0006362927944363831051, 0.4836123550491836509, 0.2008762815993576367 ) ) ;
#21613 = CARTESIAN_POINT ( 'NONE',  ( -0.09842519685039370636, 0.07874015748031495954, 0.04546065111729331171 ) ) ;
#21614 = EDGE_LOOP ( 'NONE', ( #7847, #24379 ) ) ;
#21615 = CARTESIAN_POINT ( 'NONE',  ( -0.4010740433761567081, 0.000000000000000000, -0.2342519685039370358 ) ) ;
#21616 = ( CONVERSION_BASED_UNIT ( 'INCH', #19064 ) LENGTH_UNIT ( ) NAMED_UNIT ( #10878 ) ) ;
#21617 = ORIENTED_EDGE ( 'NONE', *, *, #24672, .F. ) ;
#21618 = CARTESIAN_POINT ( 'NONE',  ( -0.1580799066051628565, -0.4326553680327470675, 0.1639447408228894565 ) ) ;
#21619 = CARTESIAN_POINT ( 'NONE',  ( -0.4848217985909654137, 0.000000000000000000, -0.05511811023622047168 ) ) ;
#21620 = CARTESIAN_POINT ( 'NONE',  ( -0.4165721057576322606, 0.3313508221749649763, 0.1322834645669291320 ) ) ;
#21621 = VERTEX_POINT ( 'NONE', #27852 ) ;
#21622 = CARTESIAN_POINT ( 'NONE',  ( -0.5511811023622047445, -0.03607471876259067678, 0.9202755905511811330 ) ) ;
#21623 = DIRECTION ( 'NONE',  ( -0.6234898018587330393, 0.7818314824680302477, 0.000000000000000000 ) ) ;
#21624 = VERTEX_POINT ( 'NONE', #2131 ) ;
#21625 = CIRCLE ( 'NONE', #26552, 0.4807043897637795493 ) ;
#21626 = CARTESIAN_POINT ( 'NONE',  ( -0.1771653543307086520, -5.663984251968503442E-18, -0.1673228346456692994 ) ) ;
#21627 = PRESENTATION_STYLE_ASSIGNMENT (( #23894 ) ) ;
#21628 = AXIS2_PLACEMENT_3D ( 'NONE', #24811, #20723, #25096 ) ;
#21629 = CIRCLE ( 'NONE', #15338, 0.1771653543307086798 ) ;
#21630 = CARTESIAN_POINT ( 'NONE',  ( 0.1516263115863346334, -0.2937912646890007973, -0.3972688187320929099 ) ) ;
#21631 = CARTESIAN_POINT ( 'NONE',  ( 0.000000000000000000, 0.000000000000000000, 0.01181102362204724393 ) ) ;
#21632 = CARTESIAN_POINT ( 'NONE',  ( 0.1522836969735571200, 0.4941010236220468865, -0.01864847287710777804 ) ) ;
#21633 = EDGE_CURVE ( 'NONE', #15505, #24639, #21417, .T. ) ;
#21634 = DIRECTION ( 'NONE',  ( 0.000000000000000000, 1.000000000000000000, 0.000000000000000000 ) ) ;
#21635 = FACE_OUTER_BOUND ( 'NONE', #17350, .T. ) ;
#21636 = CARTESIAN_POINT ( 'NONE',  ( 0.5724622793726006353, -0.3313001865994052442, 0.1616495878854405099 ) ) ;
#21637 = AXIS2_PLACEMENT_3D ( 'NONE', #26032, #27005, #1015 ) ;
#21638 = DIRECTION ( 'NONE',  ( 0.4999999999999997780, -0.8660254037844388186, 0.000000000000000000 ) ) ;
#21639 = CARTESIAN_POINT ( 'NONE',  ( 0.1109424284362303254, 0.2012500529900838608, 0.000000000000000000 ) ) ;
#21640 = EDGE_CURVE ( 'NONE', #22985, #4548, #11790, .T. ) ;
#21641 = DIRECTION ( 'NONE',  ( 0.9009688679024191460, 0.4338837391175580094, 0.000000000000000000 ) ) ;
#21642 = B_SPLINE_CURVE_WITH_KNOTS ( 'NONE', 3,
 ( #8217, #8360, #27149, #5677, #16692, #14297, #1424, #16534, #10040, #23054 ),
 .UNSPECIFIED., .F., .F.,
 ( 4, 2, 2, 2, 4 ),
 ( 0.000000000000000000, 0.2499999999999998335, 0.4999999999999996669, 0.7499999999999997780, 1.000000000000000000 ),
 .UNSPECIFIED. ) ;
#21643 = CARTESIAN_POINT ( 'NONE',  ( 0.4539000224941021067, -0.3482225189666773302, 0.9399606299212598381 ) ) ;
#21644 = DIRECTION ( 'NONE',  ( 0.000000000000000000, 0.000000000000000000, -1.000000000000000000 ) ) ;
#21645 = ORIENTED_EDGE ( 'NONE', *, *, #5625, .F. ) ;
#21646 = CARTESIAN_POINT ( 'NONE',  ( -0.1584813376850940092, 0.3213059197594776428, -3.115157480314961980 ) ) ;
#21647 = EDGE_CURVE ( 'NONE', #13891, #1203, #5006, .T. ) ;
#21648 = VERTEX_POINT ( 'NONE', #26399 ) ;
#21649 = ORIENTED_EDGE ( 'NONE', *, *, #23182, .T. ) ;
#21650 = CIRCLE ( 'NONE', #16686, 0.7874015748031496509 ) ;
#21651 = ORIENTED_EDGE ( 'NONE', *, *, #1132, .F. ) ;
#21652 = CARTESIAN_POINT ( 'NONE',  ( 0.06699507805605696420, 0.5085118447796661556, -1.550196850393700920 ) ) ;
#21653 = CARTESIAN_POINT ( 'NONE',  ( -0.4121125639592903012, -0.2386018002122738402, 0.1212655228592417339 ) ) ;
#21654 = CARTESIAN_POINT ( 'NONE',  ( 0.000000000000000000, 0.000000000000000000, -3.278217716535432842E-17 ) ) ;
#21655 = VERTEX_POINT ( 'NONE', #20048 ) ;
#21656 = FACE_OUTER_BOUND ( 'NONE', #17115, .T. ) ;
#21657 = VERTEX_POINT ( 'NONE', #11296 ) ;
#21658 = CARTESIAN_POINT ( 'NONE',  ( -0.5118110236220472231, 3.201384367575308305E-17, 1.766732283464566899 ) ) ;
#21659 = CARTESIAN_POINT ( 'NONE',  ( 0.0007595033562148819414, 0.6881885572739390167, 0.3401574803149606252 ) ) ;
#21660 = CARTESIAN_POINT ( 'NONE',  ( 0.4246272423003497609, 0.5071139714522435726, 0.1926811207740559140 ) ) ;
#21661 = CONICAL_SURFACE ( 'NONE', #21201, 0.3135473077061334268, 0.2617993874999994808 ) ;
#21662 = CARTESIAN_POINT ( 'NONE',  ( -0.3039508883504944969, 0.000000000000000000, -0.1111195235210984261 ) ) ;
#21663 = EDGE_CURVE ( 'NONE', #25476, #1804, #22608, .T. ) ;
#21664 = VECTOR ( 'NONE', #18471, 39.37007874015748143 ) ;
#21665 = DIRECTION ( 'NONE',  ( 1.000000000000000000, 0.000000000000000000, 0.000000000000000000 ) ) ;
#21666 = ORIENTED_EDGE ( 'NONE', *, *, #3710, .T. ) ;
#21667 = DIRECTION ( 'NONE',  ( 0.000000000000000000, 1.000000000000000000, 0.000000000000000000 ) ) ;
#21668 = EDGE_CURVE ( 'NONE', #22807, #21106, #10897, .T. ) ;
#21669 = CARTESIAN_POINT ( 'NONE',  ( 0.4351030398461776527, -0.1477428134820240602, -1.928289503579159625 ) ) ;
#21670 = CARTESIAN_POINT ( 'NONE',  ( 0.4351030398461604998, 0.1477428134820414352, -1.928289503579168951 ) ) ;
#21671 = AXIS2_PLACEMENT_3D ( 'NONE', #15835, #22335, #2962 ) ;
#21672 = PRODUCT_CONTEXT ( 'NONE', #3649, 'mechanical' ) ;
#21673 = DIRECTION ( 'NONE',  ( 0.000000000000000000, 0.000000000000000000, -1.000000000000000000 ) ) ;
#21674 = LINE ( 'NONE', #17424, #11241 ) ;
#21675 = EDGE_CURVE ( 'NONE', #23587, #22315, #26209, .T. ) ;
#21676 = ORIENTED_EDGE ( 'NONE', *, *, #13114, .F. ) ;
#21677 = CARTESIAN_POINT ( 'NONE',  ( -0.6262477747318130339, -0.06831769653862618252, -0.2390583512122653465 ) ) ;
#21678 = DIRECTION ( 'NONE',  ( 0.000000000000000000, 0.000000000000000000, 1.000000000000000000 ) ) ;
#21679 = CARTESIAN_POINT ( 'NONE',  ( 0.3512268162760113777, -0.4004221243553278131, 1.747047244094488194 ) ) ;
#21680 = PLANE ( 'NONE',  #4832 ) ;
#21681 = VERTEX_POINT ( 'NONE', #13407 ) ;
#21682 = EDGE_CURVE ( 'NONE', #13237, #16707, #1863, .T. ) ;
#21683 = AXIS2_PLACEMENT_3D ( 'NONE', #22415, #15653, #19882 ) ;
#21684 = CARTESIAN_POINT ( 'NONE',  ( -0.0006681923949046837848, 0.6336721034123411478, 0.1061598535668189930 ) ) ;
#21685 = CARTESIAN_POINT ( 'NONE',  ( -0.1570092758121678089, -0.4330450457732858416, 0.1771653543307084855 ) ) ;
#21686 = VERTEX_POINT ( 'NONE', #699 ) ;
#21687 = CARTESIAN_POINT ( 'NONE',  ( 0.4157391792961063204, 0.3323952789219082882, 0.3401574803149606252 ) ) ;
#21688 = VERTEX_POINT ( 'NONE', #24155 ) ;
#21689 = CARTESIAN_POINT ( 'NONE',  ( -0.0003454908279975297527, 0.3771652360013086902, 0.1992142436757342316 ) ) ;
#21690 = VERTEX_POINT ( 'NONE', #16097 ) ;
#21691 = AXIS2_PLACEMENT_3D ( 'NONE', #3749, #27211, #25082 ) ;
#21692 = CARTESIAN_POINT ( 'NONE',  ( 0.09590060490395689585, 0.2273032555864669124, 0.000000000000000000 ) ) ;
#21693 = DIRECTION ( 'NONE',  ( -0.000000000000000000, -1.000000000000000000, -0.000000000000000000 ) ) ;
#21694 = CARTESIAN_POINT ( 'NONE',  ( 0.4954156765914815574, -0.2860899518037339773, 0.9399606299212598381 ) ) ;
#21695 = FACE_OUTER_BOUND ( 'NONE', #9423, .T. ) ;
#21696 = CARTESIAN_POINT ( 'NONE',  ( 1.687505431895960050E-16, 0.4724409448818896462, -1.377952755905512472 ) ) ;
#21697 = CARTESIAN_POINT ( 'NONE',  ( 0.4417502570507448323, -0.05811937031602956022, -1.934055118110236116 ) ) ;
#21698 = EDGE_CURVE ( 'NONE', #12220, #17730, #18374, .T. ) ;
#21699 = CARTESIAN_POINT ( 'NONE',  ( 0.02438677169350735724, -0.3726024258163779246, -3.115157480314960647 ) ) ;
#21700 = CARTESIAN_POINT ( 'NONE',  ( 0.6751968503937006982, 8.268776616290199217E-17, -0.01377952755905511792 ) ) ;
#21701 = LINE ( 'NONE', #2735, #21429 ) ;
#21702 = DIRECTION ( 'NONE',  ( 0.000000000000000000, 0.000000000000000000, -1.000000000000000000 ) ) ;
#21703 = EDGE_CURVE ( 'NONE', #14646, #5816, #2740, .T. ) ;
#21704 = ORIENTED_EDGE ( 'NONE', *, *, #26242, .F. ) ;
#21705 = CARTESIAN_POINT ( 'NONE',  ( -0.4055118110236220486, 4.966087413865251393E-17, -1.639108858267716421E-17 ) ) ;
#21706 = VECTOR ( 'NONE', #9936, 39.37007874015748854 ) ;
#21707 = DIRECTION ( 'NONE',  ( 0.000000000000000000, 0.000000000000000000, 1.000000000000000000 ) ) ;
#21708 = VERTEX_POINT ( 'NONE', #4787 ) ;
#21709 = ORIENTED_EDGE ( 'NONE', *, *, #2816, .F. ) ;
#21710 = DIRECTION ( 'NONE',  ( 0.000000000000000000, -1.000000000000000000, 0.000000000000000000 ) ) ;
#21711 = CARTESIAN_POINT ( 'NONE',  ( -0.1339654526248285626, 0.4984899526255159308, 1.766732283464566899 ) ) ;
#21712 = CARTESIAN_POINT ( 'NONE',  ( -0.03349795313264326141, 0.5118110236220472231, 1.766732283464566899 ) ) ;
#21713 = CARTESIAN_POINT ( 'NONE',  ( -0.1327036767659760530, 0.4954415918530867269, 1.747047244094488194 ) ) ;
#21714 = CARTESIAN_POINT ( 'NONE',  ( -1.692913385826771533, 0.07874015748031495954, -1.036610629921259805E-16 ) ) ;
#21715 = ORIENTED_EDGE ( 'NONE', *, *, #20565, .F. ) ;
#21716 = ORIENTED_EDGE ( 'NONE', *, *, #7551, .F. ) ;
#21717 = CARTESIAN_POINT ( 'NONE',  ( 0.1151913129404419367, -0.3392387706403586223, -3.115157480314960647 ) ) ;
#21718 = EDGE_LOOP ( 'NONE', ( #21065, #2391 ) ) ;
#21719 = CARTESIAN_POINT ( 'NONE',  ( -0.5383630292499967940, 0.4286833100733393742, 0.3401591245381555551 ) ) ;
#21720 = LENGTH_MEASURE_WITH_UNIT ( LENGTH_MEASURE( 0.02539999999999999897 ), #20242 ) ;
#21721 = CARTESIAN_POINT ( 'NONE',  ( 0.2952755905264887182, 0.000000000000000000, -2.322834645648386154 ) ) ;
#21722 = CARTESIAN_POINT ( 'NONE',  ( 0.3007905576423755556, -0.1482986320106471911, 1.953740157480315043 ) ) ;
#21723 = VERTEX_POINT ( 'NONE', #24419 ) ;
#21724 = EDGE_CURVE ( 'NONE', #16188, #285, #4574, .T. ) ;
#21725 = AXIS2_PLACEMENT_3D ( 'NONE', #24350, #24483, #2861 ) ;
#21726 = DIRECTION ( 'NONE',  ( 1.000000000000000000, 0.000000000000000000, 0.000000000000000000 ) ) ;
#21727 = ORIENTED_EDGE ( 'NONE', *, *, #7937, .F. ) ;
#21728 = ORIENTED_EDGE ( 'NONE', *, *, #11372, .F. ) ;
#21729 = VERTEX_POINT ( 'NONE', #2667 ) ;
#21730 = CARTESIAN_POINT ( 'NONE',  ( -0.1643029338971332409, -0.4497088275964746806, 0.08349695147668606543 ) ) ;
#21731 = AXIS2_PLACEMENT_3D ( 'NONE', #6461, #4599, #6744 ) ;
#21732 = CIRCLE ( 'NONE', #24410, 0.7500000000000001110 ) ;
#21733 = B_SPLINE_CURVE_WITH_KNOTS ( 'NONE', 3,
 ( #13415, #2677, #5514, #22316 ),
 .UNSPECIFIED., .F., .F.,
 ( 4, 4 ),
 ( 0.2305109203526903294, 0.2318252341354939960 ),
 .UNSPECIFIED. ) ;
#21734 = CONTEXT_DEPENDENT_SHAPE_REPRESENTATION ( #9964, #11864 ) ;
#21735 = ADVANCED_FACE ( 'NONE', ( #13545 ), #6386, .T. ) ;
#21736 = CARTESIAN_POINT ( 'NONE',  ( -2.685748425196850164E-17, 0.000000000000000000, -3.115157480314960647 ) ) ;
#21737 = DIRECTION ( 'NONE',  ( -1.000000000000000000, 0.000000000000000000, 0.000000000000000000 ) ) ;
#21738 = CARTESIAN_POINT ( 'NONE',  ( 0.03937007874015749365, 0.06819097667593998491, -0.3779527559055118058 ) ) ;
#21739 = ORIENTED_EDGE ( 'NONE', *, *, #17953, .T. ) ;
#21740 = ITEM_DEFINED_TRANSFORMATION ( 'NONE', 'NONE', #21097,  #11588 ) ;
#21741 = CARTESIAN_POINT ( 'NONE',  ( -0.0006479495459697725245, 0.5014297259258653217, 0.3080453759641655909 ) ) ;
#21742 = AXIS2_PLACEMENT_3D ( 'NONE', #18971, #12193, #16439 ) ;
#21743 = CARTESIAN_POINT ( 'NONE',  ( -0.3615656011995883046, -1.111062966736172219, -0.3994379734395031578 ) ) ;
#21744 = LINE ( 'NONE', #25426, #20497 ) ;
#21745 = CYLINDRICAL_SURFACE ( 'NONE', #12385, 0.07874015748031489015 ) ;
#21746 = CARTESIAN_POINT ( 'NONE',  ( -0.0001924259990424426062, 0.4692913385826772976, 0.07637549214372836570 ) ) ;
#21747 = AXIS2_PLACEMENT_3D ( 'NONE', #15734, #13883, #22218 ) ;
#21748 = ADVANCED_FACE ( 'NONE', ( #7193 ), #26666, .T. ) ;
#21749 = FACE_OUTER_BOUND ( 'NONE', #9862, .T. ) ;
#21750 = EDGE_LOOP ( 'NONE', ( #14144, #2489, #576 ) ) ;
#21751 = CARTESIAN_POINT ( 'NONE',  ( -0.2956505864974143805, 0.3532288989643738719, 0.1771653543307089018 ) ) ;
#21752 = CARTESIAN_POINT ( 'NONE',  ( 0.3520570504767833175, -0.04632170870443329952, 1.953740157480315487 ) ) ;
#21753 = ORIENTED_EDGE ( 'NONE', *, *, #25951, .F. ) ;
#21754 = CARTESIAN_POINT ( 'NONE',  ( -0.4792984784067314541, 0.08391448672285535537, 0.1827409795192550812 ) ) ;
#21755 = EDGE_CURVE ( 'NONE', #3938, #21621, #5208, .T. ) ;
#21756 = CARTESIAN_POINT ( 'NONE',  ( 0.000000000000000000, 0.000000000000000000, -0.1559029880880275776 ) ) ;
#21757 = CARTESIAN_POINT ( 'NONE',  ( -0.1968503937007874127, 5.332515748031495785E-18, 0.09092130223458683158 ) ) ;
#21758 = ADVANCED_FACE ( 'NONE', ( #20329 ), #8845, .F. ) ;
#21759 = CARTESIAN_POINT ( 'NONE',  ( -0.5708661417322835607, 0.000000000000000000, 0.000000000000000000 ) ) ;
#21760 = VERTEX_POINT ( 'NONE', #10691 ) ;
#21761 = CARTESIAN_POINT ( 'NONE',  ( 0.03607471876262385857, -0.5511811023622048555, 0.9202755905511811330 ) ) ;
#21762 = EDGE_CURVE ( 'NONE', #13221, #13188, #9515, .T. ) ;
#21763 = CARTESIAN_POINT ( 'NONE',  ( 0.6202606299212598540, 0.08876456692913387014, 1.087052427674648014E-17 ) ) ;
#21764 = ORIENTED_EDGE ( 'NONE', *, *, #21126, .T. ) ;
#21765 = CARTESIAN_POINT ( 'NONE',  ( 0.2243804351505061800, 0.2666304421188489537, 0.1166443193913617588 ) ) ;
#21766 = AXIS2_PLACEMENT_3D ( 'NONE', #10460, #27715, #23623 ) ;
#21767 = EDGE_CURVE ( 'NONE', #20284, #16979, #12688, .T. ) ;
#21768 = DIRECTION ( 'NONE',  ( 0.000000000000000000, 0.000000000000000000, -1.000000000000000000 ) ) ;
#21769 = CARTESIAN_POINT ( 'NONE',  ( -0.0005789221761214173069, 0.4692909815006417462, 0.07637795275590551769 ) ) ;
#21770 = CARTESIAN_POINT ( 'NONE',  ( 0.1136811023622047168, -1.315836188112323537E-17, -0.09679133858267717494 ) ) ;
#21771 = CARTESIAN_POINT ( 'NONE',  ( 0.6397637795275591399, 0.000000000000000000, -0.7480314960629921295 ) ) ;
#21772 = DIRECTION ( 'NONE',  ( 0.000000000000000000, 0.000000000000000000, -1.000000000000000000 ) ) ;
#21773 = CARTESIAN_POINT ( 'NONE',  ( -0.07874015748031495954, -0.04546065111729338803, -0.4724409448818898127 ) ) ;
#21774 = ORIENTED_EDGE ( 'NONE', *, *, #26156, .T. ) ;
#21775 = CARTESIAN_POINT ( 'NONE',  ( -0.09139240964747707974, -0.07874015748031501505, -0.02109836160874977232 ) ) ;
#21776 = CARTESIAN_POINT ( 'NONE',  ( 0.5526079293737076181, -0.1480156394741905801, 0.9399606299212598381 ) ) ;
#21777 = DIRECTION ( 'NONE',  ( 1.000000000000000000, 0.000000000000000000, 0.000000000000000000 ) ) ;
#21778 = CARTESIAN_POINT ( 'NONE',  ( -0.1968503937007874127, -0.07874015748031495954, -0.04546065111729331171 ) ) ;
#21779 = CIRCLE ( 'NONE', #15040, 0.6889763779527560139 ) ;
#21780 = CIRCLE ( 'NONE', #9572, 1.288838582677165556 ) ;
#21781 = ORIENTED_EDGE ( 'NONE', *, *, #14553, .F. ) ;
#21782 = ADVANCED_FACE ( 'NONE', ( #17468 ), #26082, .F. ) ;
#21783 = CIRCLE ( 'NONE', #1939, 0.1181102362204718703 ) ;
#21784 = DIRECTION ( 'NONE',  ( 0.000000000000000000, -1.000000000000000000, 0.000000000000000000 ) ) ;
#21785 = DIRECTION ( 'NONE',  ( 0.000000000000000000, 0.000000000000000000, -1.000000000000000000 ) ) ;
#21786 = LINE ( 'NONE', #4139, #2860 ) ;
#21787 = CARTESIAN_POINT ( 'NONE',  ( 0.3411065095061437402, 0.06065137456822566192, 0.1377952755905510474 ) ) ;
#21788 = EDGE_CURVE ( 'NONE', #13641, #27702, #13578, .T. ) ;
#21789 = CARTESIAN_POINT ( 'NONE',  ( -0.2358179517456306662, 0.2802411498293116421, 0.1910323753015176762 ) ) ;
#21790 = EDGE_LOOP ( 'NONE', ( #11285, #25893, #16591, #24939, #16449 ) ) ;
#21791 = VERTEX_POINT ( 'NONE', #4737 ) ;
#21792 = CARTESIAN_POINT ( 'NONE',  ( 0.000000000000000000, 0.000000000000000000, -0.1377952755905511861 ) ) ;
#21793 = CARTESIAN_POINT ( 'NONE',  ( 0.7283464566929135353, 0.000000000000000000, 0.01181102362204724393 ) ) ;
#21794 = DIRECTION ( 'NONE',  ( 0.000000000000000000, 0.000000000000000000, 1.000000000000000000 ) ) ;
#21795 = B_SPLINE_CURVE_WITH_KNOTS ( 'NONE', 3,
 ( #4446, #618, #23936, #6704 ),
 .UNSPECIFIED., .F., .F.,
 ( 4, 4 ),
 ( 1.217380381967462011, 1.219305002860847864 ),
 .UNSPECIFIED. ) ;
#21796 = CIRCLE ( 'NONE', #23160, 0.01377952755905510404 ) ;
#21797 = ( NAMED_UNIT ( * ) SI_UNIT ( $, .STERADIAN. ) SOLID_ANGLE_UNIT ( ) ) ;
#21798 = VECTOR ( 'NONE', #10462, 39.37007874015748143 ) ;
#21799 = CYLINDRICAL_SURFACE ( 'NONE', #21362, 0.3937007874015748254 ) ;
#21800 = EDGE_LOOP ( 'NONE', ( #21146, #3006, #8810, #2503, #6569 ) ) ;
#21801 = CARTESIAN_POINT ( 'NONE',  ( 0.08582157620924656116, 0.3030878557544539054, -3.598143271073415139 ) ) ;
#21802 = CARTESIAN_POINT ( 'NONE',  ( -0.2180862235769562008, -0.4423390553432419714, -1.569881889763779625 ) ) ;
#21803 = ADVANCED_FACE ( 'NONE', ( #23840 ), #8634, .F. ) ;
#21804 = CARTESIAN_POINT ( 'NONE',  ( 0.4585215200179055817, -0.03001016326913584151, -1.928289503579156516 ) ) ;
#21805 = CIRCLE ( 'NONE', #9600, 0.1771653543307086520 ) ;
#21806 = CARTESIAN_POINT ( 'NONE',  ( 0.000000000000000000, 0.000000000000000000, -0.2342519685039370358 ) ) ;
#21807 = AXIS2_PLACEMENT_3D ( 'NONE', #24291, #18191, #11301 ) ;
#21808 = CARTESIAN_POINT ( 'NONE',  ( -0.3661417322834645272, -0.4724409448818898127, 0.8182917201112815953 ) ) ;
#21809 = AXIS2_PLACEMENT_3D ( 'NONE', #5031, #13650, #3317 ) ;
#21810 = CARTESIAN_POINT ( 'NONE',  ( -0.0006362927944366116549, 0.4836123550488269363, 0.2008762816006358365 ) ) ;
#21811 = CARTESIAN_POINT ( 'NONE',  ( -0.6505662911506299162, -0.02047472615278346855, 0.2361156911274059078 ) ) ;
#21812 = DIRECTION ( 'NONE',  ( 0.000000000000000000, 0.000000000000000000, 1.000000000000000000 ) ) ;
#21813 = ( NAMED_UNIT ( * ) SI_UNIT ( $, .STERADIAN. ) SOLID_ANGLE_UNIT ( ) ) ;
#21814 = AXIS2_PLACEMENT_3D ( 'NONE', #25942, #22212, #6595 ) ;
#21815 = ADVANCED_FACE ( 'NONE', ( #19862 ), #2341, .F. ) ;
#21816 = AXIS2_PLACEMENT_3D ( 'NONE', #3024, #9116, #653 ) ;
#21817 = TOROIDAL_SURFACE ( 'NONE', #12777, 0.1476377952755905387, 0.01968503937007873988 ) ;
#21818 = DIRECTION ( 'NONE',  ( 0.000000000000000000, 1.000000000000000000, 0.000000000000000000 ) ) ;
#21819 = EDGE_LOOP ( 'NONE', ( #16820, #4113, #12245, #6878, #1308, #17473 ) ) ;
#21820 = CARTESIAN_POINT ( 'NONE',  ( 0.4160174684701755665, 0.3320469875258716397, 0.3401599409343964431 ) ) ;
#21821 = EDGE_CURVE ( 'NONE', #23853, #3232, #19448, .T. ) ;
#21822 = ORIENTED_EDGE ( 'NONE', *, *, #21493, .F. ) ;
#21823 = CARTESIAN_POINT ( 'NONE',  ( -0.6806799598997224088, 0.07848646696189429117, 0.07615904174712244401 ) ) ;
#21824 = EDGE_LOOP ( 'NONE', ( #16656, #24248 ) ) ;
#21825 = AXIS2_PLACEMENT_3D ( 'NONE', #14248, #3478, #12391 ) ;
#21826 = CARTESIAN_POINT ( 'NONE',  ( -0.4417361510194242613, -0.05819755867303597063, -1.934055118110236338 ) ) ;
#21827 = CARTESIAN_POINT ( 'NONE',  ( -0.07217847769028858107, -0.04546065111729339497, -5.567324087794789421E-18 ) ) ;
#21828 = CARTESIAN_POINT ( 'NONE',  ( 3.616083068348477018E-17, 0.9055118110236217710, 0.2952755905511805223 ) ) ;
#21829 = DIRECTION ( 'NONE',  ( 0.000000000000000000, 0.000000000000000000, -1.000000000000000000 ) ) ;
#21830 = CIRCLE ( 'NONE', #24529, 0.05216535433070866590 ) ;
#21831 = DIRECTION ( 'NONE',  ( -0.000000000000000000, -1.000000000000000000, -0.000000000000000000 ) ) ;
#21832 = ADVANCED_FACE ( 'NONE', ( #19727 ), #8712, .T. ) ;
#21833 = CARTESIAN_POINT ( 'NONE',  ( 0.2937497900415150243, -0.3350145293469216079, -1.934055118110236560 ) ) ;
#21834 = CARTESIAN_POINT ( 'NONE',  ( -0.2462256503455939050, 0.2807137536170327685, -3.115157480314960647 ) ) ;
#21835 = FACE_OUTER_BOUND ( 'NONE', #21458, .T. ) ;
#21836 = CARTESIAN_POINT ( 'NONE',  ( 0.1522836969735573143, 0.2938892803217905692, 0.3971963147566898167 ) ) ;
#21837 = CONICAL_SURFACE ( 'NONE', #6517, 0.3726024258163779246, 0.2617993874999969828 ) ;
#21838 = EDGE_CURVE ( 'NONE', #4552, #25079, #15226, .T. ) ;
#21839 = ORIENTED_EDGE ( 'NONE', *, *, #24019, .T. ) ;
#21840 = DIRECTION ( 'NONE',  ( -0.9396926207859082059, 0.3420201433256691015, 0.000000000000000000 ) ) ;
#21841 = AXIS2_PLACEMENT_3D ( 'NONE', #27304, #16422, #14314 ) ;
#21842 = AXIS2_PLACEMENT_3D ( 'NONE', #18954, #2004, #17125 ) ;
#21843 = ORIENTED_EDGE ( 'NONE', *, *, #16043, .T. ) ;
#21844 = AXIS2_PLACEMENT_3D ( 'NONE', #23373, #6136, #16562 ) ;
#21845 = EDGE_LOOP ( 'NONE', ( #1795, #8459, #15165, #23700, #4252, #20693 ) ) ;
#21846 = CARTESIAN_POINT ( 'NONE',  ( 0.5190862322091315262, -0.1177929122753177127, 0.3401574803149606252 ) ) ;
#21847 = CARTESIAN_POINT ( 'NONE',  ( -0.4055118110236220486, 0.9448818897637796255, -0.1771653543307086520 ) ) ;
#21848 = CYLINDRICAL_SURFACE ( 'NONE', #11149, 0.6614173228346456046 ) ;
#21849 = PLANE ( 'NONE',  #5470 ) ;
#21850 = ORIENTED_EDGE ( 'NONE', *, *, #8864, .T. ) ;
#21851 = CARTESIAN_POINT ( 'NONE',  ( 0.3606853515406215904, 0.09660931395005435685, -3.115157480314960647 ) ) ;
#21852 = CARTESIAN_POINT ( 'NONE',  ( 0.000000000000000000, 0.000000000000000000, 0.2362204724409449064 ) ) ;
#21853 = ORIENTED_EDGE ( 'NONE', *, *, #3828, .T. ) ;
#21854 = DIRECTION ( 'NONE',  ( 0.000000000000000000, 0.000000000000000000, 1.000000000000000000 ) ) ;
#21855 = CARTESIAN_POINT ( 'NONE',  ( 0.000000000000000000, 0.4692913385826771866, 0.03818897637795275884 ) ) ;
#21856 = ADVANCED_FACE ( 'NONE', ( #519 ), #15377, .T. ) ;
#21857 = CARTESIAN_POINT ( 'NONE',  ( -0.1078280746903930304, -0.3175540113612211890, 1.953740157480315043 ) ) ;
#21858 = ORIENTED_EDGE ( 'NONE', *, *, #13683, .F. ) ;
#21859 = EDGE_LOOP ( 'NONE', ( #13084, #6892, #27343, #8817, #6293, #18905 ) ) ;
#21860 = ORIENTED_EDGE ( 'NONE', *, *, #3257, .T. ) ;
#21861 = ADVANCED_FACE ( 'NONE', ( #10971, #17601 ), #21849, .T. ) ;
#21862 = CARTESIAN_POINT ( 'NONE',  ( 0.3268939675028499914, -0.1881330340946397728, 0.1992125984251968684 ) ) ;
#21863 = CARTESIAN_POINT ( 'NONE',  ( 0.5869493968174713805, 0.4267795242930089161, 0.000000000000000000 ) ) ;
#21864 = ORIENTED_EDGE ( 'NONE', *, *, #14504, .T. ) ;
#21865 = ORIENTED_EDGE ( 'NONE', *, *, #17812, .T. ) ;
#21866 = EDGE_LOOP ( 'NONE', ( #27064, #15312, #9388, #10664 ) ) ;
#21867 = CARTESIAN_POINT ( 'NONE',  ( -0.1610509776512594748, -0.4407912692718567449, 0.1992125984251968684 ) ) ;
#21868 = CIRCLE ( 'NONE', #7005, 0.01181102362204724046 ) ;
#21869 = B_SPLINE_CURVE_WITH_KNOTS ( 'NONE', 3,
 ( #16331, #13926, #20705, #14221, #12364, #10101 ),
 .UNSPECIFIED., .F., .F.,
 ( 4, 2, 4 ),
 ( 0.4045103800602309896, 0.4064350009536160102, 0.4083596218470010308 ),
 .UNSPECIFIED. ) ;
#21870 = FACE_OUTER_BOUND ( 'NONE', #17958, .T. ) ;
#21871 = AXIS2_PLACEMENT_3D ( 'NONE', #12658, #18729, #10675 ) ;
#21872 = DIRECTION ( 'NONE',  ( 0.000000000000000000, 0.000000000000000000, 1.000000000000000000 ) ) ;
#21873 = ORIENTED_EDGE ( 'NONE', *, *, #5090, .T. ) ;
#21874 = DIRECTION ( 'NONE',  ( 0.000000000000000000, 0.000000000000000000, 1.000000000000000000 ) ) ;
#21875 = LINE ( 'NONE', #25839, #3773 ) ;
#21876 = MANIFOLD_SOLID_BREP ( 'b14500x', #26760 ) ;
#21877 = AXIS2_PLACEMENT_3D ( 'NONE', #6053, #12537, #10688 ) ;
#21878 = CARTESIAN_POINT ( 'NONE',  ( -0.0006345105826668660581, 0.4803145415259079121, 0.2362204724409446843 ) ) ;
#21879 = EDGE_CURVE ( 'NONE', #19812, #12596, #27169, .T. ) ;
#21880 = PLANE ( 'NONE',  #9391 ) ;
#21881 = CARTESIAN_POINT ( 'NONE',  ( 0.000000000000000000, 0.000000000000000000, -0.01377952755905511792 ) ) ;
#21882 = DIRECTION ( 'NONE',  ( 0.000000000000000000, 0.000000000000000000, 1.000000000000000000 ) ) ;
#21883 = SURFACE_STYLE_FILL_AREA ( #4632 ) ;
#21884 = AXIS2_PLACEMENT_3D ( 'NONE', #19304, #363, #7778 ) ;
#21885 = FACE_BOUND ( 'NONE', #2364, .T. ) ;
#21886 = ORIENTED_EDGE ( 'NONE', *, *, #5056, .F. ) ;
#21887 = CIRCLE ( 'NONE', #8347, 0.09842519685039370636 ) ;
#21888 = VERTEX_POINT ( 'NONE', #9818 ) ;
#21889 = CARTESIAN_POINT ( 'NONE',  ( 0.03532354024591839031, -0.6299212598425196763, 0.5531496062992127261 ) ) ;
#21890 = CARTESIAN_POINT ( 'NONE',  ( 0.3543307086614173040, -0.02325840746512450319, 1.953740157480314821 ) ) ;
#21891 = B_SPLINE_CURVE_WITH_KNOTS ( 'NONE', 3,
 ( #4533, #2538, #570, #8899, #11161, #4660, #23897, #4792, #19779, #15427 ),
 .UNSPECIFIED., .F., .F.,
 ( 4, 2, 2, 2, 4 ),
 ( 0.000000000000000000, 0.2499999999999996669, 0.4999999999999997780, 0.7499999999999998890, 1.000000000000000000 ),
 .UNSPECIFIED. ) ;
#21892 = ORIENTED_EDGE ( 'NONE', *, *, #3729, .T. ) ;
#21893 = CARTESIAN_POINT ( 'NONE',  ( -0.3765118517642104257, 2.305470170520414967E-17, -3.100567304031763172 ) ) ;
#21894 = CARTESIAN_POINT ( 'NONE',  ( -0.4889536969035324643, 0.06441834428466573781, -1.569881889763779625 ) ) ;
#21895 = DIRECTION ( 'NONE',  ( 0.000000000000000000, 0.000000000000000000, -1.000000000000000000 ) ) ;
#21896 = DIRECTION ( 'NONE',  ( 0.000000000000000000, 1.000000000000000000, 0.000000000000000000 ) ) ;
#21897 = ORIENTED_EDGE ( 'NONE', *, *, #4995, .T. ) ;
#21898 = CARTESIAN_POINT ( 'NONE',  ( -0.5230301363771709955, 0.1775991818008312573, 0.9399606299212598381 ) ) ;
#21899 = DIMENSIONAL_EXPONENTS ( 1.000000000000000000, 0.000000000000000000, 0.000000000000000000, 0.000000000000000000, 0.000000000000000000, 0.000000000000000000, 0.000000000000000000 ) ;
#21900 = AXIS2_PLACEMENT_3D ( 'NONE', #11345, #11203, #2305 ) ;
#21901 = CARTESIAN_POINT ( 'NONE',  ( 0.3606049308157521227, 0.06410376196636191626, 0.1910323753053202456 ) ) ;
#21902 = ORIENTED_EDGE ( 'NONE', *, *, #233, .F. ) ;
#21903 = FACE_OUTER_BOUND ( 'NONE', #25613, .T. ) ;
#21904 = CARTESIAN_POINT ( 'NONE',  ( -0.6233907401648717261, -0.4658374228745700285, -0.9954608982700638986 ) ) ;
#21905 = DIRECTION ( 'NONE',  ( 0.000000000000000000, 0.000000000000000000, -1.000000000000000000 ) ) ;
#21906 = DIRECTION ( 'NONE',  ( -0.9790454724845842893, -0.1018208755700882318, 0.1763589297585410332 ) ) ;
#21907 = DIRECTION ( 'NONE',  ( 0.9848077530122081313, 0.1736481776669301369, -0.000000000000000000 ) ) ;
#21908 = APPLICATION_CONTEXT ( 'automotive_design' ) ;
#21909 = VECTOR ( 'NONE', #12331, 39.37007874015748143 ) ;
#21910 = CARTESIAN_POINT ( 'NONE',  ( 0.000000000000000000, 0.6102362204724409711, 0.4724409448818898127 ) ) ;
#21911 = CARTESIAN_POINT ( 'NONE',  ( 0.4925073816753560152, 0.08623502184910394885, 0.1259302777096748815 ) ) ;
#21912 = VECTOR ( 'NONE', #3425, 39.37007874015748143 ) ;
#21913 = EDGE_CURVE ( 'NONE', #8592, #1325, #7269, .T. ) ;
#21914 = EDGE_CURVE ( 'NONE', #5544, #10703, #14529, .T. ) ;
#21915 = CARTESIAN_POINT ( 'NONE',  ( -0.5118110236220472231, 3.201384367575308305E-17, 1.766732283464566899 ) ) ;
#21916 = EDGE_CURVE ( 'NONE', #16707, #13237, #17469, .T. ) ;
#21917 = CARTESIAN_POINT ( 'NONE',  ( 0.4300830224589536899, -0.3772436174784755680, 0.9399606299212598381 ) ) ;
#21918 = PRODUCT_RELATED_PRODUCT_CATEGORY ( 'part', '', ( #24947 ) ) ;
#21919 = DIRECTION ( 'NONE',  ( 1.000000000000000000, 0.000000000000000000, 0.000000000000000000 ) ) ;
#21920 = EDGE_LOOP ( 'NONE', ( #17161, #6395, #15415, #18138 ) ) ;
#21921 = DIRECTION ( 'NONE',  ( 0.000000000000000000, -1.000000000000000000, 0.000000000000000000 ) ) ;
#21922 = EDGE_CURVE ( 'NONE', #16783, #23339, #20159, .T. ) ;
#21923 = AXIS2_PLACEMENT_3D ( 'NONE', #8816, #17431, #366 ) ;
#21924 = ORIENTED_EDGE ( 'NONE', *, *, #4679, .F. ) ;
#21925 = ADVANCED_FACE ( 'NONE', ( #20415 ), #2746, .F. ) ;
#21926 = MANIFOLD_SOLID_BREP ( 'ISO 4762 M5x16 Socket Head Cap Screw', #19107 ) ;
#21927 = ORIENTED_EDGE ( 'NONE', *, *, #24777, .T. ) ;
#21928 = CARTESIAN_POINT ( 'NONE',  ( 0.6055690743987126590, -0.5162970762339605946, 6.322814960629921339E-17 ) ) ;
#21929 = AXIS2_PLACEMENT_3D ( 'NONE', #13283, #9297, #448 ) ;
#21930 = CARTESIAN_POINT ( 'NONE',  ( 0.4620947063919693121, 0.08187111969648641630, 0.07637630773773071424 ) ) ;
#21931 = CARTESIAN_POINT ( 'NONE',  ( 0.5018154743079163982, -0.1152098006149074177, 0.1473214333276229582 ) ) ;
#21932 = CARTESIAN_POINT ( 'NONE',  ( 0.5981657849660177995, 0.000000000000000000, 0.000000000000000000 ) ) ;
#21933 = VERTEX_POINT ( 'NONE', #13778 ) ;
#21934 = CARTESIAN_POINT ( 'NONE',  ( -4.618943439303797186E-17, -0.3771653543307086909, 0.07637795275590551769 ) ) ;
#21935 = EDGE_LOOP ( 'NONE', ( #17142, #3248, #10028, #19614 ) ) ;
#21936 = AXIS2_PLACEMENT_3D ( 'NONE', #26052, #17299, #13383 ) ;
#21937 = DIRECTION ( 'NONE',  ( 0.000000000000000000, 0.000000000000000000, 1.000000000000000000 ) ) ;
#21938 = B_SPLINE_CURVE_WITH_KNOTS ( 'NONE', 3,
 ( #22650, #11768, #20672, #12053, #13892, #1326, #5272, #20390, #24759, #16163, #11914, #763, #24613, #22228, #9495, #5562, #5422, #13609, #14041, #18091, #26456, #9354, #2991, #24472, #7119, #16016, #11624, #7247, #1192, #15866, #20247, #14187, #15742, #4987 ),
 .UNSPECIFIED., .F., .F.,
 ( 4, 2, 2, 2, 2, 2, 2, 2, 2, 2, 2, 2, 2, 2, 2, 2, 4 ),
 ( 0.5000000000000000000, 0.5312500000000000000, 0.5624999999999998890, 0.5937499999999998890, 0.6249999999999998890, 0.6562499999999998890, 0.6874999999999997780, 0.7187499999999997780, 0.7499999999999997780, 0.7812499999999997780, 0.8124999999999998890, 0.8437499999999998890, 0.8749999999999998890, 0.9062500000000000000, 0.9375000000000000000, 0.9687500000000000000, 1.000000000000000000 ),
 .UNSPECIFIED. ) ;
#21939 = DIRECTION ( 'NONE',  ( -1.000000000000000000, 0.000000000000000000, 0.000000000000000000 ) ) ;
#21940 = CARTESIAN_POINT ( 'NONE',  ( 0.3339160553493882300, 1.241955529277656956, -0.7081600496628898123 ) ) ;
#21941 = CARTESIAN_POINT ( 'NONE',  ( 0.000000000000000000, 0.000000000000000000, 0.1377952755905511861 ) ) ;
#21942 = DIRECTION ( 'NONE',  ( 0.000000000000000000, -1.000000000000000000, 0.000000000000000000 ) ) ;
#21943 = ORIENTED_EDGE ( 'NONE', *, *, #11263, .F. ) ;
#21944 = DIRECTION ( 'NONE',  ( 1.000000000000000000, 0.000000000000000000, 0.000000000000000000 ) ) ;
#21945 = CARTESIAN_POINT ( 'NONE',  ( -0.4423390553432507977, -0.2180862235769348567, -1.569881889763779625 ) ) ;
#21946 = B_SPLINE_CURVE_WITH_KNOTS ( 'NONE', 3,
 ( #18941, #1712, #3682, #10175 ),
 .UNSPECIFIED., .F., .F.,
 ( 4, 4 ),
 ( 0.3881911340211371408, 0.3898838371647120327 ),
 .UNSPECIFIED. ) ;
#21947 = CARTESIAN_POINT ( 'NONE',  ( 0.4351030398461604998, 0.1477428134820414352, -1.928289503579168951 ) ) ;
#21948 = ORIENTED_EDGE ( 'NONE', *, *, #16459, .F. ) ;
#21949 = FACE_OUTER_BOUND ( 'NONE', #27671, .T. ) ;
#21950 = AXIS2_PLACEMENT_3D ( 'NONE', #5383, #9601, #16124 ) ;
#21951 = CARTESIAN_POINT ( 'NONE',  ( -0.5614173959463371055, 0.4467232815834303872, 0.1601585119451258976 ) ) ;
#21952 = CARTESIAN_POINT ( 'NONE',  ( -0.03001016326913591784, 0.4585215200179055817, -1.928289503579156516 ) ) ;
#21953 = ADVANCED_FACE ( 'NONE', ( #17986, #26622 ), #15896, .T. ) ;
#21954 = AXIS2_PLACEMENT_3D ( 'NONE', #10622, #17669, #17404 ) ;
#21955 = EDGE_CURVE ( 'NONE', #3160, #21729, #7599, .T. ) ;
#21956 = CARTESIAN_POINT ( 'NONE',  ( -0.4771018889076559244, 0.3804760601893846794, 0.2362204724409449064 ) ) ;
#21957 = SURFACE_STYLE_USAGE ( .BOTH. , #23533 ) ;
#21958 = CARTESIAN_POINT ( 'NONE',  ( -0.4790936880892668892, 0.08507591033002856462, 0.1827409795186053509 ) ) ;
#21959 = DIRECTION ( 'NONE',  ( 0.000000000000000000, -1.000000000000000000, 0.000000000000000000 ) ) ;
#21960 = CARTESIAN_POINT ( 'NONE',  ( -0.1623262587462485640, -0.4476804331104035084, 0.2330651858513022867 ) ) ;
#21961 = CARTESIAN_POINT ( 'NONE',  ( 0.4162944719209866196, 0.3316996361851579089, 0.3401599409343964431 ) ) ;
#21962 = CARTESIAN_POINT ( 'NONE',  ( 0.5511811023622047445, 3.414809992080329023E-17, 0.9202755905511811330 ) ) ;
#21963 = CARTESIAN_POINT ( 'NONE',  ( 0.000000000000000000, 0.000000000000000000, -0.01377952755905511792 ) ) ;
#21964 = ORIENTED_EDGE ( 'NONE', *, *, #45, .T. ) ;
#21965 = CARTESIAN_POINT ( 'NONE',  ( -0.4303822302053990634, -0.1152775731717099322, -1.934055118110236338 ) ) ;
#21966 = CARTESIAN_POINT ( 'NONE',  ( -4.618943439303797186E-17, -0.3771653543307086909, -3.278217716535432842E-17 ) ) ;
#21967 = DIRECTION ( 'NONE',  ( 0.000000000000000000, 1.000000000000000000, 0.000000000000000000 ) ) ;
#21968 = CARTESIAN_POINT ( 'NONE',  ( 0.0005789383928823483780, 0.4762008496965042803, 0.1212655228852155959 ) ) ;
#21969 = DIRECTION ( 'NONE',  ( 0.000000000000000000, 0.000000000000000000, -1.000000000000000000 ) ) ;
#21970 = CARTESIAN_POINT ( 'NONE',  ( 0.2836590635674519634, 0.2488091035917033567, -3.100567304031761395 ) ) ;
#21971 = CARTESIAN_POINT ( 'NONE',  ( 0.4055118110236220486, 0.000000000000000000, 0.3543307086614173040 ) ) ;
#21972 = CARTESIAN_POINT ( 'NONE',  ( 0.0007595033562148819414, 0.6881885572739390167, 0.1322834645669291320 ) ) ;
#21973 = CARTESIAN_POINT ( 'NONE',  ( 0.000000000000000000, 0.03937007874015751446, 0.000000000000000000 ) ) ;
#21974 = ORIENTED_EDGE ( 'NONE', *, *, #12795, .T. ) ;
#21975 = CARTESIAN_POINT ( 'NONE',  ( -0.4417361510194065533, 0.05819755867303653962, -1.934055118110236338 ) ) ;
#21976 = ADVANCED_FACE ( 'NONE', ( #8407 ), #9802, .T. ) ;
#21977 = EDGE_CURVE ( 'NONE', #7423, #17871, #14367, .T. ) ;
#21978 = ORIENTED_EDGE ( 'NONE', *, *, #20768, .F. ) ;
#21979 = CARTESIAN_POINT ( 'NONE',  ( 8.353478384051541640E-17, 8.115082136941410961E-18, 0.1023622047244094474 ) ) ;
#21980 = CARTESIAN_POINT ( 'NONE',  ( 0.4472135058506040983, 0.2577577458591219783, 1.766732283464566899 ) ) ;
#21981 = PRODUCT_CONTEXT ( 'NONE', #614, 'mechanical' ) ;
#21982 = CARTESIAN_POINT ( 'NONE',  ( -0.4856708409200499732, 0.1649135259616961724, 1.747047244094488194 ) ) ;
#21983 = EDGE_CURVE ( 'NONE', #290, #2628, #18350, .T. ) ;
#21984 = ORIENTED_EDGE ( 'NONE', *, *, #11351, .T. ) ;
#21985 = CARTESIAN_POINT ( 'NONE',  ( 0.3412792617076850221, 0.05967164814832588010, 0.1377952755905512139 ) ) ;
#21986 = ORIENTED_EDGE ( 'NONE', *, *, #8529, .F. ) ;
#21987 = ORIENTED_EDGE ( 'NONE', *, *, #26539, .F. ) ;
#21989 = CARTESIAN_POINT ( 'NONE',  ( -0.3535721684717733071, -0.1200583359873110406, -3.115157480314960647 ) ) ;
#21988 = CARTESIAN_POINT ( 'NONE',  ( 0.5614173959472870123, 0.4467232815841902793, 0.3122824329351960304 ) ) ;
#21990 = ORIENTED_EDGE ( 'NONE', *, *, #3710, .F. ) ;
#21991 = DIRECTION ( 'NONE',  ( -0.4999999999999995004, -0.8660254037844390407, 0.000000000000000000 ) ) ;
#21992 = FACE_OUTER_BOUND ( 'NONE', #23724, .T. ) ;
#21993 = CARTESIAN_POINT ( 'NONE',  ( 0.1482986320106562672, -0.3007905576423960392, 1.953740157480315043 ) ) ;
#21994 = EDGE_CURVE ( 'NONE', #214, #10335, #14505, .T. ) ;
#21995 = ORIENTED_EDGE ( 'NONE', *, *, #8917, .F. ) ;
#21996 = ORIENTED_EDGE ( 'NONE', *, *, #19297, .F. ) ;
#21997 = CARTESIAN_POINT ( 'NONE',  ( 0.3265485372158890010, -0.1887320510662011952, 0.1992150590373740204 ) ) ;
#21998 = DIRECTION ( 'NONE',  ( 0.000000000000000000, 1.000000000000000000, 0.000000000000000000 ) ) ;
#21999 = ORIENTED_EDGE ( 'NONE', *, *, #23563, .F. ) ;
#22000 = CARTESIAN_POINT ( 'NONE',  ( -0.1648275707511323573, -0.4857079805364574177, -1.550196850393701142 ) ) ;
#22001 = ORIENTED_EDGE ( 'NONE', *, *, #15691, .F. ) ;
#22002 = ORIENTED_EDGE ( 'NONE', *, *, #22244, .F. ) ;
#22003 = CARTESIAN_POINT ( 'NONE',  ( 0.07874015748031480688, 0.1968503937007873850, -3.558522530913132531 ) ) ;
#22004 = ( GEOMETRIC_REPRESENTATION_CONTEXT ( 3 ) GLOBAL_UNCERTAINTY_ASSIGNED_CONTEXT ( ( #5441 ) ) GLOBAL_UNIT_ASSIGNED_CONTEXT ( ( #19, #23301, #25821 ) ) REPRESENTATION_CONTEXT ( 'NONE', 'WORKASPACE' ) ) ;
#22005 = CARTESIAN_POINT ( 'NONE',  ( 0.01027864967365997931, 0.1968503937007874127, -3.193894829389441359 ) ) ;
#22006 = AXIS2_PLACEMENT_3D ( 'NONE', #15623, #24488, #24087 ) ;
#22007 = CARTESIAN_POINT ( 'NONE',  ( 0.09842519685039355370, 0.2165354330708661457, -3.548228346456693050 ) ) ;
#22008 = EDGE_LOOP ( 'NONE', ( #1485, #21843, #8652, #17580 ) ) ;
#22009 = PRODUCT_DEFINITION_SHAPE ( 'NONE', 'NONE',  #27918 ) ;
#22010 = ADVANCED_FACE ( 'NONE', ( #23108 ), #18841, .F. ) ;
#22011 = DIRECTION ( 'NONE',  ( 0.000000000000000000, 1.000000000000000000, 0.000000000000000000 ) ) ;
#22012 = CARTESIAN_POINT ( 'NONE',  ( -0.3429980251342298336, -0.09187177619659059324, 1.953740157480315043 ) ) ;
#22013 = EDGE_CURVE ( 'NONE', #3515, #22576, #3454, .T. ) ;
#22014 = CARTESIAN_POINT ( 'NONE',  ( -0.5738137315987272835, 1.106933345739570473, 0.07395176699327656034 ) ) ;
#22015 = CARTESIAN_POINT ( 'NONE',  ( -0.3631207844635358506, -1.104178130233240296, -0.3878391952755386729 ) ) ;
#22016 = CARTESIAN_POINT ( 'NONE',  ( -0.3998447049182496382, 0.4754871227240771714, 0.09685039370078740717 ) ) ;
#22017 = DIRECTION ( 'NONE',  ( 0.000000000000000000, 0.000000000000000000, 1.000000000000000000 ) ) ;
#22018 = DIRECTION ( 'NONE',  ( 1.000000000000000000, 0.000000000000000000, 0.000000000000000000 ) ) ;
#22019 = CARTESIAN_POINT ( 'NONE',  ( 0.06699507805369657454, 0.5085118447801424413, 1.766732283464566899 ) ) ;
#22020 = AXIS2_PLACEMENT_3D ( 'NONE', #23903, #15789, #8770 ) ;
#22021 = CARTESIAN_POINT ( 'NONE',  ( 0.4327133464945798758, -0.2505177833311500457, 0.1259302777204239776 ) ) ;
#22022 = ORIENTED_EDGE ( 'NONE', *, *, #5186, .T. ) ;
#22023 = TOROIDAL_SURFACE ( 'NONE', #2162, 0.5915354330708662012, 0.05216535433070866590 ) ;
#22024 = DIRECTION ( 'NONE',  ( -1.000000000000000000, 0.000000000000000000, 0.000000000000000000 ) ) ;
#22025 = CARTESIAN_POINT ( 'NONE',  ( 0.000000000000000000, 0.3937007873309092409, 0.000000000000000000 ) ) ;
#22026 = ORIENTED_EDGE ( 'NONE', *, *, #21054, .T. ) ;
#22027 = DIRECTION ( 'NONE',  ( 0.000000000000000000, -1.000000000000000000, 0.000000000000000000 ) ) ;
#22028 = DIRECTION ( 'NONE',  ( 0.2036417511401760472, 0.9790454724845841783, 0.000000000000000000 ) ) ;
#22029 = CIRCLE ( 'NONE', #21596, 0.5379714048901780288 ) ;
#22030 = ORIENTED_EDGE ( 'NONE', *, *, #6126, .T. ) ;
#22031 = ORIENTED_EDGE ( 'NONE', *, *, #21788, .T. ) ;
#22032 = DIRECTION ( 'NONE',  ( 0.000000000000000000, 0.000000000000000000, 1.000000000000000000 ) ) ;
#22033 = ORIENTED_EDGE ( 'NONE', *, *, #25062, .T. ) ;
#22034 = DIRECTION ( 'NONE',  ( 0.000000000000000000, 0.000000000000000000, 1.000000000000000000 ) ) ;
#22035 = CARTESIAN_POINT ( 'NONE',  ( 0.000000000000000000, 0.000000000000000000, 0.3059055118110236560 ) ) ;
#22036 = FACE_OUTER_BOUND ( 'NONE', #20074, .T. ) ;
#22037 = CARTESIAN_POINT ( 'NONE',  ( 0.3905379133858267737, -0.2805118110236220486, 0.4858607088160724063 ) ) ;
#22038 = CARTESIAN_POINT ( 'NONE',  ( 0.3543307086614173596, 0.000000000000000000, 1.953740157480315043 ) ) ;
#22039 = CIRCLE ( 'NONE', #9854, 0.1308464566929133932 ) ;
#22040 = CARTESIAN_POINT ( 'NONE',  ( -0.4246272423007197983, 0.5071139714526793352, 0.1926811207703575390 ) ) ;
#22041 = AXIS2_PLACEMENT_3D ( 'NONE', #19120, #27469, #17149 ) ;
#22042 = EDGE_CURVE ( 'NONE', #11528, #12477, #5589, .T. ) ;
#22043 = DIRECTION ( 'NONE',  ( 1.000000000000000000, 0.000000000000000000, 0.000000000000000000 ) ) ;
#22044 = CARTESIAN_POINT ( 'NONE',  ( 0.5671862884094760471, 0.07472527936312113594, 0.9399606299212598381 ) ) ;
#22045 = CARTESIAN_POINT ( 'NONE',  ( 0.000000000000000000, 0.000000000000000000, 0.1322834645669291320 ) ) ;
#22046 = AXIS2_PLACEMENT_3D ( 'NONE', #15482, #4316, #9090 ) ;
#22047 = DIRECTION ( 'NONE',  ( -1.000000000000000000, 0.000000000000000000, 0.000000000000000000 ) ) ;
#22048 = ORIENTED_EDGE ( 'NONE', *, *, #17260, .T. ) ;
#22049 = MANIFOLD_SOLID_BREP ( 'Deep Groove Ball Bearing 20x37x9', #12801 ) ;
#22050 = VERTEX_POINT ( 'NONE', #18993 ) ;
#22051 = CONICAL_SURFACE ( 'NONE', #13, 0.08582677165393072516, 0.7853981625000011624 ) ;
#22052 = CARTESIAN_POINT ( 'NONE',  ( 0.000000000000000000, 0.6881889763779527325, 0.4062992125984251635 ) ) ;
#22053 = FACE_BOUND ( 'NONE', #20827, .T. ) ;
#22054 = CIRCLE ( 'NONE', #3083, 0.5007874015748031704 ) ;
#22055 = VERTEX_POINT ( 'NONE', #3885 ) ;
#22056 = CARTESIAN_POINT ( 'NONE',  ( 0.000000000000000000, 0.000000000000000000, 0.01181102362204724393 ) ) ;
#22057 = ORIENTED_EDGE ( 'NONE', *, *, #13358, .F. ) ;
#22058 = ADVANCED_FACE ( 'NONE', ( #1759 ), #4391, .T. ) ;
#22059 = CARTESIAN_POINT ( 'NONE',  ( 0.0007595033562148819414, 0.6881885572739390167, 0.3401574803149606252 ) ) ;
#22060 = AXIS2_PLACEMENT_3D ( 'NONE', #16568, #5712, #21095 ) ;
#22061 = CARTESIAN_POINT ( 'NONE',  ( 0.6867658503616472787, -0.1559616964381364546, 0.1443310008642350595 ) ) ;
#22062 = CARTESIAN_POINT ( 'NONE',  ( 0.7873253891977465280, 0.3482478513048458124, 0.02382806990687684479 ) ) ;
#22063 = CARTESIAN_POINT ( 'NONE',  ( 0.000000000000000000, 0.000000000000000000, 0.3401574803149606252 ) ) ;
#22064 = CARTESIAN_POINT ( 'NONE',  ( -0.5190862322091315262, -0.1177929122753175184, 0.1322834645669291320 ) ) ;
#22065 = ADVANCED_FACE ( 'NONE', ( #21264 ), #2593, .F. ) ;
#22066 = EDGE_LOOP ( 'NONE', ( #26125, #21113, #8140, #3647 ) ) ;
#22067 = CARTESIAN_POINT ( 'NONE',  ( 0.006552947699234559081, 0.3149606299212598381, -3.646653543307086576 ) ) ;
#22068 = CARTESIAN_POINT ( 'NONE',  ( 0.1638952246732497953, -0.2749627978706437048, -0.4762495361032456631 ) ) ;
#22069 = CARTESIAN_POINT ( 'NONE',  ( -0.1585706980422225409, -0.4669911931914833558, -1.550196850393700920 ) ) ;
#22070 = CARTESIAN_POINT ( 'NONE',  ( 0.4555658499975999698, -0.06001958459475366381, -1.928289503579165398 ) ) ;
#22071 = ORIENTED_EDGE ( 'NONE', *, *, #12766, .F. ) ;
#22072 = CARTESIAN_POINT ( 'NONE',  ( 0.2796934465393767222, -0.3645739570812915331, -1.928289503579138753 ) ) ;
#22073 = DIRECTION ( 'NONE',  ( -1.000000000000000000, 0.000000000000000000, 0.000000000000000000 ) ) ;
#22074 = AXIS2_PLACEMENT_3D ( 'NONE', #18588, #14681, #21151 ) ;
#22075 = CARTESIAN_POINT ( 'NONE',  ( -0.5791695622050556658, 0.4608640948048334796, 0.2161412452746097335 ) ) ;
#22076 = CARTESIAN_POINT ( 'NONE',  ( 0.06001958459474798779, 0.4555658499976080189, -1.928289503579158515 ) ) ;
#22077 = CARTESIAN_POINT ( 'NONE',  ( 0.2303471512294322787, -0.4798602677570401598, 0.3401574803149606252 ) ) ;
#22078 = ORIENTED_EDGE ( 'NONE', *, *, #2778, .F. ) ;
#22079 = ORIENTED_EDGE ( 'NONE', *, *, #26746, .F. ) ;
#22080 = LINE ( 'NONE', #6841, #11951 ) ;
#22081 = DIRECTION ( 'NONE',  ( 0.000000000000000000, -1.000000000000000000, 0.000000000000000000 ) ) ;
#22082 = CARTESIAN_POINT ( 'NONE',  ( 0.4563908000639787521, 1.076366897322332816, -0.3413933471944003428 ) ) ;
#22083 = DIRECTION ( 'NONE',  ( 1.000000000000000000, 0.000000000000000000, 0.000000000000000000 ) ) ;
#22084 = FACE_OUTER_BOUND ( 'NONE', #17277, .T. ) ;
#22085 = CARTESIAN_POINT ( 'NONE',  ( -0.1579154690107267833, -0.4355388305873471588, 0.2048502515406250557 ) ) ;
#22086 = ORIENTED_EDGE ( 'NONE', *, *, #12519, .F. ) ;
#22087 = FACE_OUTER_BOUND ( 'NONE', #8106, .T. ) ;
#22088 = VERTEX_POINT ( 'NONE', #4703 ) ;
#22089 = CIRCLE ( 'NONE', #20751, 0.7283464566929134243 ) ;
#22090 = CARTESIAN_POINT ( 'NONE',  ( -0.6633461167951516524, 0.02596910924942653909, 0.2360419752028775631 ) ) ;
#22091 = ORIENTED_EDGE ( 'NONE', *, *, #7586, .T. ) ;
#22092 = ADVANCED_FACE ( 'NONE', ( #17430, #9078 ), #21680, .T. ) ;
#22093 = CARTESIAN_POINT ( 'NONE',  ( -0.4446020952038907681, 0.000000000000000000, -1.934055118110236338 ) ) ;
#22094 = FACE_OUTER_BOUND ( 'NONE', #9536, .T. ) ;
#22095 = VECTOR ( 'NONE', #17047, 39.37007874015748143 ) ;
#22096 = ORIENTED_EDGE ( 'NONE', *, *, #15759, .F. ) ;
#22097 = CARTESIAN_POINT ( 'NONE',  ( -0.6751968503937006982, 0.000000000000000000, -0.01377952755905511792 ) ) ;
#22098 = ADVANCED_FACE ( 'NONE', ( #26046 ), #6232, .F. ) ;
#22099 = SPHERICAL_SURFACE ( 'NONE', #2304, 0.1003956692913385851 ) ;
#22100 = CARTESIAN_POINT ( 'NONE',  ( 0.0005710523241079800989, 0.4632828964885310485, 0.1494804572073301641 ) ) ;
#22101 = ADVANCED_FACE ( 'NONE', ( #2184, #12775 ), #12912, .T. ) ;
#22102 = ORIENTED_EDGE ( 'NONE', *, *, #25291, .T. ) ;
#22103 = CARTESIAN_POINT ( 'NONE',  ( 0.000000000000000000, 0.000000000000000000, 0.9055118110027171596 ) ) ;
#22104 = CARTESIAN_POINT ( 'NONE',  ( -0.2296683860596825943, 0.2993674444872254092, -3.100567304031761395 ) ) ;
#22105 = EDGE_CURVE ( 'NONE', #5917, #11793, #6706, .T. ) ;
#22106 = DIRECTION ( 'NONE',  ( 1.000000000000000000, 0.000000000000000000, 0.000000000000000000 ) ) ;
#22107 = CARTESIAN_POINT ( 'NONE',  ( 0.3131893444311545371, 0.3723335979429350795, 0.1075369453526922314 ) ) ;
#22108 = CARTESIAN_POINT ( 'NONE',  ( 0.6512499169099681406, 0.1155267097730202641, 0.1616495878900666150 ) ) ;
#22109 = ORIENTED_EDGE ( 'NONE', *, *, #4559, .T. ) ;
#22110 = FACE_OUTER_BOUND ( 'NONE', #6208, .T. ) ;
#22111 = AXIS2_PLACEMENT_3D ( 'NONE', #20957, #25188, #1459 ) ;
#22112 = CARTESIAN_POINT ( 'NONE',  ( 0.4585215200179057482, 0.06002032661671145852, -1.928289503579156960 ) ) ;
#22113 = AXIS2_PLACEMENT_3D ( 'NONE', #26529, #3075, #9294 ) ;
#22114 = ORIENTED_EDGE ( 'NONE', *, *, #8421, .T. ) ;
#22115 = DIRECTION ( 'NONE',  ( 0.000000000000000000, 0.000000000000000000, -1.000000000000000000 ) ) ;
#22116 = CARTESIAN_POINT ( 'NONE',  ( -0.3121994997598253052, -0.4069448477556119048, 1.747047244094488194 ) ) ;
#22117 = DIRECTION ( 'NONE',  ( 0.000000000000000000, 1.000000000000000000, 0.000000000000000000 ) ) ;
#22118 = EDGE_LOOP ( 'NONE', ( #14557, #1748 ) ) ;
#22119 = STYLED_ITEM ( 'NONE', ( #9484 ), #11975 ) ;
#22120 = CARTESIAN_POINT ( 'NONE',  ( 0.3726024258163779246, 0.02438677169350801990, -3.115157480314960647 ) ) ;
#22121 = CARTESIAN_POINT ( 'NONE',  ( -0.7874015748031496509, 0.6226544199590670070, -0.5245967315940827103 ) ) ;
#22122 = CARTESIAN_POINT ( 'NONE',  ( 0.0004405150045870399964, 0.6212597256746514862, 0.09684874924366457249 ) ) ;
#22124 = VERTEX_POINT ( 'NONE', #14925 ) ;
#22125 = CARTESIAN_POINT ( 'NONE',  ( -0.1677079028045287967, 0.2904160862623510475, 1.953740157480315043 ) ) ;
#22126 = ORIENTED_EDGE ( 'NONE', *, *, #21698, .T. ) ;
#22127 = EDGE_LOOP ( 'NONE', ( #23642, #6821 ) ) ;
#22128 = ADVANCED_FACE ( 'NONE', ( #2579 ), #24068, .F. ) ;
#22129 = CYLINDRICAL_SURFACE ( 'NONE', #25407, 0.6299212598425196763 ) ;
#22130 = VERTEX_POINT ( 'NONE', #15343 ) ;
#22131 = B_SPLINE_CURVE_WITH_KNOTS ( 'NONE', 3,
 ( #19731, #8579, #15506, #23708, #14960, #2620, #11242, #6464, #4208, #15097 ),
 .UNSPECIFIED., .F., .F.,
 ( 4, 2, 2, 2, 4 ),
 ( 0.000000000000000000, 0.2500000000000000000, 0.5000000000000000000, 0.7500000000000000000, 1.000000000000000000 ),
 .UNSPECIFIED. ) ;
#22132 = ORIENTED_EDGE ( 'NONE', *, *, #26276, .F. ) ;
#22133 = ORIENTED_EDGE ( 'NONE', *, *, #6736, .T. ) ;
#22134 = DIRECTION ( 'NONE',  ( 0.000000000000000000, 1.000000000000000000, 0.000000000000000000 ) ) ;
#22135 = EDGE_CURVE ( 'NONE', #1348, #13865, #4882, .T. ) ;
#22136 = DIRECTION ( 'NONE',  ( 1.000000000000000000, 0.000000000000000000, 0.000000000000000000 ) ) ;
#22137 = DIRECTION ( 'NONE',  ( 0.000000000000000000, 1.000000000000000000, 0.000000000000000000 ) ) ;
#22138 = DIRECTION ( 'NONE',  ( 1.000000000000000000, 0.000000000000000000, 0.000000000000000000 ) ) ;
#22139 = FACE_OUTER_BOUND ( 'NONE', #3960, .T. ) ;
#22140 = CARTESIAN_POINT ( 'NONE',  ( 0.07870736637777360489, 0.2165354330708661457, -3.212150913388296836 ) ) ;
#22141 = MANIFOLD_SOLID_BREP ( 'Shaft Seal 15x26x7', #18170 ) ;
#22142 = CARTESIAN_POINT ( 'NONE',  ( -0.3429980251342297226, 0.09187177619658862260, 1.953740157480315043 ) ) ;
#22143 = DIRECTION ( 'NONE',  ( 1.000000000000000000, 0.000000000000000000, 0.000000000000000000 ) ) ;
#22144 = LENGTH_MEASURE_WITH_UNIT ( LENGTH_MEASURE( 0.02539999999999999897 ), #19053 ) ;
#22145 = DIRECTION ( 'NONE',  ( 0.000000000000000000, 0.000000000000000000, 1.000000000000000000 ) ) ;
#22146 = CARTESIAN_POINT ( 'NONE',  ( 0.1522836969735573143, -0.1970374587079582740, -0.4531137400369409374 ) ) ;
#22147 = CARTESIAN_POINT ( 'NONE',  ( 0.000000000000000000, 0.000000000000000000, 0.1771653543307086520 ) ) ;
#22148 = DIRECTION ( 'NONE',  ( 0.000000000000000000, 0.000000000000000000, -1.000000000000000000 ) ) ;
#22149 = CARTESIAN_POINT ( 'NONE',  ( 0.3382184156732163660, 0.3855916753051394363, 1.766732283464566899 ) ) ;
#22150 = AXIS2_PLACEMENT_3D ( 'NONE', #17042, #14940, #12654 ) ;
#22151 = CARTESIAN_POINT ( 'NONE',  ( 0.03008364706454716778, -0.2273032555864669124, 2.185478346456692557E-17 ) ) ;
#22152 = CARTESIAN_POINT ( 'NONE',  ( 0.3777066424207166095, 0.3020248451656780131, 0.2008762815943767877 ) ) ;
#22153 = ORIENTED_EDGE ( 'NONE', *, *, #8214, .T. ) ;
#22154 = EDGE_LOOP ( 'NONE', ( #21216, #23566, #6079, #8724 ) ) ;
#22155 = CARTESIAN_POINT ( 'NONE',  ( -0.2313841235333771451, 0.3010840436257776198, -3.100567304031763172 ) ) ;
#22156 = AXIS2_PLACEMENT_3D ( 'NONE', #23705, #26217, #15094 ) ;
#22157 = ORIENTED_EDGE ( 'NONE', *, *, #23162, .T. ) ;
#22158 = EDGE_CURVE ( 'NONE', #14806, #18478, #16579, .T. ) ;
#22159 = PRESENTATION_LAYER_ASSIGNMENT (  '', '', ( #6388 ) ) ;
#22160 = CYLINDRICAL_SURFACE ( 'NONE', #11572, 0.3722026523000413478 ) ;
#22161 = DIRECTION ( 'NONE',  ( 1.000000000000000000, 0.000000000000000000, 0.000000000000000000 ) ) ;
#22162 = AXIS2_PLACEMENT_3D ( 'NONE', #190, #441, #19359 ) ;
#22163 = ORIENTED_EDGE ( 'NONE', *, *, #7834, .T. ) ;
#22164 = CARTESIAN_POINT ( 'NONE',  ( -0.5230301363771188150, -0.1775991818008711975, 0.9399606299212598381 ) ) ;
#22165 = ORIENTED_EDGE ( 'NONE', *, *, #3806, .T. ) ;
#22166 = EDGE_CURVE ( 'NONE', #12080, #13707, #20184, .T. ) ;
#22167 = CARTESIAN_POINT ( 'NONE',  ( -0.3661417322834645272, -0.4724409448818898127, -0.8182917201112815953 ) ) ;
#22168 = ORIENTED_EDGE ( 'NONE', *, *, #6354, .T. ) ;
#22169 = CARTESIAN_POINT ( 'NONE',  ( 0.000000000000000000, 0.000000000000000000, 0.01181102362204724393 ) ) ;
#22170 = CARTESIAN_POINT ( 'NONE',  ( -0.4055118110236220486, 0.9448818897637796255, -9.561468503937007847E-18 ) ) ;
#22171 = FACE_OUTER_BOUND ( 'NONE', #19997, .T. ) ;
#22172 = DIRECTION ( 'NONE',  ( 0.000000000000000000, 0.000000000000000000, 1.000000000000000000 ) ) ;
#22173 = CARTESIAN_POINT ( 'NONE',  ( -0.4339912984563299436, -0.2498791196563492356, 0.2574803149606298969 ) ) ;
#22174 = CYLINDRICAL_SURFACE ( 'NONE', #11833, 0.4226968503937005295 ) ;
#22175 = CYLINDRICAL_SURFACE ( 'NONE', #2840, 0.09842519685039370636 ) ;
#22176 = CARTESIAN_POINT ( 'NONE',  ( 0.3429980251342366060, 0.09187177619658697114, 1.953740157480315043 ) ) ;
#22177 = EDGE_CURVE ( 'NONE', #18279, #8887, #23813, .T. ) ;
#22178 = EDGE_LOOP ( 'NONE', ( #1089, #18249, #24401, #25345 ) ) ;
#22179 = DIRECTION ( 'NONE',  ( 0.000000000000000000, 0.000000000000000000, -1.000000000000000000 ) ) ;
#22180 = DIRECTION ( 'NONE',  ( 0.000000000000000000, -1.000000000000000000, 0.000000000000000000 ) ) ;
#22181 = AXIS2_PLACEMENT_3D ( 'NONE', #19220, #6374, #15003 ) ;
#22182 = PLANE ( 'NONE',  #21161 ) ;
#22183 = FACE_OUTER_BOUND ( 'NONE', #13669, .T. ) ;
#22184 = ORIENTED_EDGE ( 'NONE', *, *, #18470, .F. ) ;
#22185 = FACE_OUTER_BOUND ( 'NONE', #23824, .T. ) ;
#22186 = CARTESIAN_POINT ( 'NONE',  ( 0.000000000000000000, 0.000000000000000000, 0.1992125984251968684 ) ) ;
#22187 = EDGE_LOOP ( 'NONE', ( #17234, #2488, #25031, #6462 ) ) ;
#22188 = AXIS2_PLACEMENT_3D ( 'NONE', #9904, #1570, #18501 ) ;
#22189 = CARTESIAN_POINT ( 'NONE',  ( 0.000000000000000000, 0.9055118110236221041, 0.000000000000000000 ) ) ;
#22190 = CYLINDRICAL_SURFACE ( 'NONE', #19770, 0.2952755905511810774 ) ;
#22191 = ORIENTED_EDGE ( 'NONE', *, *, #25846, .T. ) ;
#22192 = VERTEX_POINT ( 'NONE', #6983 ) ;
#22193 = EDGE_CURVE ( 'NONE', #4851, #3160, #2193, .T. ) ;
#22194 = CARTESIAN_POINT ( 'NONE',  ( 0.1570092758121679200, -0.4330450457732857861, 0.1771653543307087630 ) ) ;
#22195 = EDGE_LOOP ( 'NONE', ( #7252, #7783 ) ) ;
#22196 = VECTOR ( 'NONE', #7676, 39.37007874015748143 ) ;
#22197 = EDGE_CURVE ( 'NONE', #2702, #14152, #9942, .T. ) ;
#22198 = DIRECTION ( 'NONE',  ( -0.000000000000000000, -0.000000000000000000, 1.000000000000000000 ) ) ;
#22199 = CARTESIAN_POINT ( 'NONE',  ( 0.7874015748031325534, 0.2970927457007063732, -0.1251225998731516909 ) ) ;
#22200 = B_SPLINE_CURVE_WITH_KNOTS ( 'NONE', 3,
 ( #19606, #6333, #25544, #12678, #4348, #21165 ),
 .UNSPECIFIED., .F., .F.,
 ( 4, 2, 4 ),
 ( 0.000000000000000000, 0.2500000000000000000, 0.5000000000000000000 ),
 .UNSPECIFIED. ) ;
#22201 = SPHERICAL_SURFACE ( 'NONE', #26111, 0.1003956692913385851 ) ;
#22202 = LINE ( 'NONE', #14015, #8732 ) ;
#22203 = ORIENTED_EDGE ( 'NONE', *, *, #12284, .F. ) ;
#22204 = CARTESIAN_POINT ( 'NONE',  ( -0.2660793235464258277, -0.2041304421298378857, 1.973425196850393970 ) ) ;
#22205 = DIRECTION ( 'NONE',  ( 0.000000000000000000, 0.000000000000000000, -1.000000000000000000 ) ) ;
#22206 = CARTESIAN_POINT ( 'NONE',  ( -0.3912931228432058872, -0.3001918266902326993, -1.550196850393700920 ) ) ;
#22207 = AXIS2_PLACEMENT_3D ( 'NONE', #7117, #15740, #9351 ) ;
#22208 = CARTESIAN_POINT ( 'NONE',  ( 0.3454440660767458815, 0.3030032861725153737, -1.928289503579147635 ) ) ;
#22209 = CARTESIAN_POINT ( 'NONE',  ( 0.06001958459476169905, -0.4555658499976140696, -1.928289503579150077 ) ) ;
#22210 = AXIS2_PLACEMENT_3D ( 'NONE', #703, #15817, #26678 ) ;
#22211 = DIRECTION ( 'NONE',  ( 1.000000000000000000, 0.000000000000000000, 0.000000000000000000 ) ) ;
#22212 = DIRECTION ( 'NONE',  ( 0.000000000000000000, 0.000000000000000000, 1.000000000000000000 ) ) ;
#22213 = DIRECTION ( 'NONE',  ( 0.000000000000000000, 0.000000000000000000, 1.000000000000000000 ) ) ;
#22214 = EDGE_CURVE ( 'NONE', #18898, #16090, #27417, .T. ) ;
#22215 = DIRECTION ( 'NONE',  ( -1.000000000000000000, 0.000000000000000000, 0.000000000000000000 ) ) ;
#22216 = AXIS2_PLACEMENT_3D ( 'NONE', #17259, #10610, #2140 ) ;
#22217 = CARTESIAN_POINT ( 'NONE',  ( -0.6165893942483189338, -0.1421421316221962716, 0.2283979491189897792 ) ) ;
#22218 = DIRECTION ( 'NONE',  ( -1.000000000000000000, 0.000000000000000000, 0.000000000000000000 ) ) ;
#22219 = CARTESIAN_POINT ( 'NONE',  ( -0.3346456692913385988, 0.000000000000000000, 2.426181102355854158 ) ) ;
#22220 = DIRECTION ( 'NONE',  ( 0.000000000000000000, 0.000000000000000000, -1.000000000000000000 ) ) ;
#22221 = ( NAMED_UNIT ( * ) PLANE_ANGLE_UNIT ( ) SI_UNIT ( $, .RADIAN. ) ) ;
#22222 = DIRECTION ( 'NONE',  ( 0.6234898018587331503, -0.7818314824680301367, 0.000000000000000000 ) ) ;
#22223 = PRODUCT_DEFINITION_SHAPE ( 'NONE', 'NONE',  #27917 ) ;
#22224 = CARTESIAN_POINT ( 'NONE',  ( 0.3339160553493882300, 0.7867001919223544082, -0.8344257386302499357 ) ) ;
#22225 = B_SPLINE_CURVE_WITH_KNOTS ( 'NONE', 2,
 ( #24159, #9166, #22038 ),
 .UNSPECIFIED., .F., .F.,
 ( 3, 3 ),
 ( 0.000000000000000000, 1.000000000000000000 ),
 .UNSPECIFIED. ) ;
#22226 = ORIENTED_EDGE ( 'NONE', *, *, #20798, .F. ) ;
#22227 = AXIS2_PLACEMENT_3D ( 'NONE', #6889, #410, #24246 ) ;
#22228 = CARTESIAN_POINT ( 'NONE',  ( -0.1141156591735126569, 0.3362580771780235844, 1.953740157480314821 ) ) ;
#22229 = ORIENTED_EDGE ( 'NONE', *, *, #21013, .T. ) ;
#22230 = CARTESIAN_POINT ( 'NONE',  ( 0.4527559054764770385, -0.02963280468032104126, -1.934055118110236338 ) ) ;
#22231 = VECTOR ( 'NONE', #26607, 39.37007874015748143 ) ;
#22232 = CARTESIAN_POINT ( 'NONE',  ( 0.0006568023596629938904, 0.5148705051067553606, 0.3251195115598493612 ) ) ;
#22233 = CARTESIAN_POINT ( 'NONE',  ( 1.692913385826771533, 0.07874015748031495954, -0.1181102362204716899 ) ) ;
#22234 = FACE_OUTER_BOUND ( 'NONE', #20165, .T. ) ;
#22235 = DIRECTION ( 'NONE',  ( 1.000000000000000000, 0.000000000000000000, 0.000000000000000000 ) ) ;
#22236 = CARTESIAN_POINT ( 'NONE',  ( -0.2602238532265429005, 0.000000000000000000, 0.07874015748031495954 ) ) ;
#22237 = CARTESIAN_POINT ( 'NONE',  ( 0.3715251363271980245, 0.06498290224717499786, 0.07637795275590551769 ) ) ;
#22238 = PLANE ( 'NONE',  #19542 ) ;
#22239 = CARTESIAN_POINT ( 'NONE',  ( 0.02464264302293732445, -0.3765118517642105367, -3.100567304031763172 ) ) ;
#22240 = DIRECTION ( 'NONE',  ( 0.9790454724845840673, -0.1018208755700883150, 0.1763589297585418658 ) ) ;
#22241 = FACE_OUTER_BOUND ( 'NONE', #10412, .T. ) ;
#22242 = ORIENTED_EDGE ( 'NONE', *, *, #25261, .T. ) ;
#22243 = CARTESIAN_POINT ( 'NONE',  ( -0.4303822302054170490, 0.1152775731717081975, -1.934055118110236338 ) ) ;
#22244 = EDGE_CURVE ( 'NONE', #12810, #22996, #3020, .T. ) ;
#22245 = CIRCLE ( 'NONE', #24471, 0.07677362204724409722 ) ;
#22246 = EDGE_CURVE ( 'NONE', #19765, #12438, #6674, .T. ) ;
#22247 = AXIS2_PLACEMENT_3D ( 'NONE', #4560, #353, #17560 ) ;
#22248 = ORIENTED_EDGE ( 'NONE', *, *, #3797, .F. ) ;
#22249 = DIRECTION ( 'NONE',  ( 0.000000000000000000, 1.000000000000000000, 0.000000000000000000 ) ) ;
#22250 = AXIS2_PLACEMENT_3D ( 'NONE', #9418, #7609, #20458 ) ;
#22251 = CARTESIAN_POINT ( 'NONE',  ( -0.5118110236220472231, -0.03349795313264326835, 1.747047244094488194 ) ) ;
#22252 = EDGE_CURVE ( 'NONE', #16370, #27302, #26060, .T. ) ;
#22253 = SURFACE_STYLE_USAGE ( .BOTH. , #5299 ) ;
#22254 = CIRCLE ( 'NONE', #4231, 0.1003956692913385573 ) ;
#22255 = CARTESIAN_POINT ( 'NONE',  ( -0.1200583359873150374, -0.3535721684717939017, -3.115157480314960647 ) ) ;
#22256 = EDGE_CURVE ( 'NONE', #22736, #26931, #7525, .T. ) ;
#22257 = CARTESIAN_POINT ( 'NONE',  ( 0.4980314960629921295, 6.183502046875907854E-17, -0.2755905511811023723 ) ) ;
#22258 = APPLICATION_CONTEXT ( 'automotive_design' ) ;
#22259 = DIRECTION ( 'NONE',  ( -1.000000000000000000, 0.000000000000000000, 0.000000000000000000 ) ) ;
#22260 = AXIS2_PLACEMENT_3D ( 'NONE', #6882, #17735, #15383 ) ;
#22261 = ORIENTED_EDGE ( 'NONE', *, *, #15982, .F. ) ;
#22262 = DIRECTION ( 'NONE',  ( 1.000000000000000000, 0.000000000000000000, 0.000000000000000000 ) ) ;
#22263 = ORIENTED_EDGE ( 'NONE', *, *, #4573, .F. ) ;
#22264 = CARTESIAN_POINT ( 'NONE',  ( 0.2938049579018460755, 0.3349573549949649842, -1.934055118110236338 ) ) ;
#22265 = ORIENTED_EDGE ( 'NONE', *, *, #17358, .T. ) ;
#22266 = EDGE_LOOP ( 'NONE', ( #9131, #6343, #1811, #8414, #11523 ) ) ;
#22267 = CARTESIAN_POINT ( 'NONE',  ( 0.000000000000000000, 0.000000000000000000, 0.3059055118110236560 ) ) ;
#22268 = CARTESIAN_POINT ( 'NONE',  ( 0.01027864967283271050, 0.1968503937007874127, -3.626965695530909972 ) ) ;
#22269 = CLOSED_SHELL ( 'NONE', ( #21324, #21069, #18072, #15762, #22968, #19407, #11405, #22456, #4942, #24417, #6906, #22661, #20691, #13517, #21758, #24347, #4029, #19123, #22445, #16361, #20860, #20380, #20634, #24179, #9136, #25390, #20697, #17203, #24135, #7678, #16741, #7341, #4008, #2302, #15009, #2728, #13480, #25266, #6397, #18653, #19525, #2287, #7493 ) ) ;
#22270 = B_SPLINE_CURVE_WITH_KNOTS ( 'NONE', 3,
 ( #15803, #26518, #834, #11556, #8886, #19903 ),
 .UNSPECIFIED., .F., .F.,
 ( 4, 2, 4 ),
 ( 0.2376120521391529850, 0.2390783382518560096, 0.2405446243645580073 ),
 .UNSPECIFIED. ) ;
#22271 = CARTESIAN_POINT ( 'NONE',  ( -0.3381532161292066796, -0.3856588814717588076, -1.550196850393701142 ) ) ;
#22272 = CARTESIAN_POINT ( 'NONE',  ( -0.03794311743615354227, 0.8811800718601279225, -0.3070871000585283506 ) ) ;
#22273 = CARTESIAN_POINT ( 'NONE',  ( 0.09842519685039370636, 0.2165354330708661457, -3.364501312335958172 ) ) ;
#22274 = CIRCLE ( 'NONE', #25901, 0.5393700787401575214 ) ;
#22275 = CARTESIAN_POINT ( 'NONE',  ( 0.000000000000000000, 0.000000000000000000, -1.550196850393700920 ) ) ;
#22276 = CARTESIAN_POINT ( 'NONE',  ( 0.08600259727896232553, 0.2165354330708660902, -3.223068997994990248 ) ) ;
#22277 = CARTESIAN_POINT ( 'NONE',  ( -0.3346456692913385988, -0.04380501567505450111, 1.973425196850393526 ) ) ;
#22278 = VECTOR ( 'NONE', #5799, 39.37007874015748854 ) ;
#22279 = DIRECTION ( 'NONE',  ( 0.000000000000000000, 1.000000000000000000, 0.000000000000000000 ) ) ;
#22280 = EDGE_CURVE ( 'NONE', #4466, #26673, #846, .T. ) ;
#22281 = CARTESIAN_POINT ( 'NONE',  ( 0.000000000000000000, 0.000000000000000000, 2.090519358671640647E-11 ) ) ;
#22282 = DIRECTION ( 'NONE',  ( 0.000000000000000000, -1.000000000000000000, 0.000000000000000000 ) ) ;
#22283 = CARTESIAN_POINT ( 'NONE',  ( 0.2355331214654129424, 0.4777261797697872625, 1.747047244094488194 ) ) ;
#22284 = EDGE_CURVE ( 'NONE', #16925, #16922, #19710, .T. ) ;
#22285 = DIRECTION ( 'NONE',  ( -0.9930684569432060016, 0.05876869877843025891, -0.1017903721789531202 ) ) ;
#22286 = CONICAL_SURFACE ( 'NONE', #12818, 0.3937007874015748254, 0.2617993874999990922 ) ;
#22287 = VERTEX_POINT ( 'NONE', #19965 ) ;
#22288 = CARTESIAN_POINT ( 'NONE',  ( 0.4061284506583976994, -0.2351468520617074898, 0.1992125984251968684 ) ) ;
#22289 = EDGE_LOOP ( 'NONE', ( #157, #4921 ) ) ;
#22290 = CARTESIAN_POINT ( 'NONE',  ( 0.2161007281672546465, -0.5956855348316323351, 0.1061598535656166492 ) ) ;
#22291 = CARTESIAN_POINT ( 'NONE',  ( 0.02325127328526765264, -0.3543292900373042342, 1.953740157480315043 ) ) ;
#22292 = ORIENTED_EDGE ( 'NONE', *, *, #15365, .T. ) ;
#22293 = CARTESIAN_POINT ( 'NONE',  ( -0.4622619257814448712, 0.08092139668561793009, 0.1992125984251968684 ) ) ;
#22294 = VERTEX_POINT ( 'NONE', #22219 ) ;
#22295 = CARTESIAN_POINT ( 'NONE',  ( -0.06441834428466709783, -0.4889536969035322977, -1.569881889763779625 ) ) ;
#22296 = ORIENTED_EDGE ( 'NONE', *, *, #11897, .T. ) ;
#22297 = EDGE_CURVE ( 'NONE', #17285, #11455, #17643, .T. ) ;
#22298 = LINE ( 'NONE', #11421, #16991 ) ;
#22299 = AXIS2_PLACEMENT_3D ( 'NONE', #17081, #16946, #23167 ) ;
#22300 = ORIENTED_EDGE ( 'NONE', *, *, #21450, .T. ) ;
#22301 = CARTESIAN_POINT ( 'NONE',  ( -0.5708661417322835607, 0.03736310157554031952, 0.9399606299212598381 ) ) ;
#22302 = EDGE_LOOP ( 'NONE', ( #25442, #3289, #19565, #7566 ) ) ;
#22303 = EDGE_LOOP ( 'NONE', ( #18895, #8279, #4595, #22395, #26163 ) ) ;
#22304 = DIRECTION ( 'NONE',  ( 0.000000000000000000, 0.000000000000000000, 1.000000000000000000 ) ) ;
#22305 = EDGE_CURVE ( 'NONE', #24688, #20284, #15330, .T. ) ;
#22306 = DIRECTION ( 'NONE',  ( 0.000000000000000000, 0.000000000000000000, 1.000000000000000000 ) ) ;
#22307 = CARTESIAN_POINT ( 'NONE',  ( -0.4355945891378961154, 0.000000000000000000, -0.2755905511811023723 ) ) ;
#22308 = CARTESIAN_POINT ( 'NONE',  ( -0.0005855335178309040850, 0.4865383137632814381, 0.2467937632985283125 ) ) ;
#22309 = DIRECTION ( 'NONE',  ( 0.000000000000000000, -1.000000000000000000, 0.000000000000000000 ) ) ;
#22310 = DIRECTION ( 'NONE',  ( 0.000000000000000000, 0.000000000000000000, 1.000000000000000000 ) ) ;
#22311 = CONICAL_SURFACE ( 'NONE', #11479, 0.3135473077061334268, 0.2617993874999994808 ) ;
#22312 = CYLINDRICAL_SURFACE ( 'NONE', #26704, 0.09842519685039378963 ) ;
#22313 = ORIENTED_EDGE ( 'NONE', *, *, #26242, .T. ) ;
#22314 = CARTESIAN_POINT ( 'NONE',  ( -0.3324885138898231451, -0.04380447413659061678, 1.953740157480315043 ) ) ;
#22315 = VERTEX_POINT ( 'NONE', #25849 ) ;
#22316 = CARTESIAN_POINT ( 'NONE',  ( 0.0005189969344232283309, 0.3771649972486724733, 0.07637795275590551769 ) ) ;
#22317 = CARTESIAN_POINT ( 'NONE',  ( -0.3073078020562972634, 0.3671449284697080873, 0.1920935997041830212 ) ) ;
#22319 = EDGE_CURVE ( 'NONE', #7047, #10159, #6500, .T. ) ;
#22318 = AXIS2_PLACEMENT_3D ( 'NONE', #10905, #26693, #18346 ) ;
#22320 = EDGE_CURVE ( 'NONE', #6811, #11452, #17235, .T. ) ;
#22321 = DIRECTION ( 'NONE',  ( 0.000000000000000000, 0.000000000000000000, 1.000000000000000000 ) ) ;
#22322 = VECTOR ( 'NONE', #16274, 39.37007874015748143 ) ;
#22323 = B_SPLINE_CURVE_WITH_KNOTS ( 'NONE', 3,
 ( #11567, #13687, #22448, #26676, #18183, #15681, #11997, #17902 ),
 .UNSPECIFIED., .F., .F.,
 ( 4, 2, 2, 4 ),
 ( 0.000000000000000000, 0.2499999999999998890, 0.4999999999999997780, 1.000000000000000000 ),
 .UNSPECIFIED. ) ;
#22324 = CARTESIAN_POINT ( 'NONE',  ( 0.000000000000000000, 0.000000000000000000, 0.01181102362204724393 ) ) ;
#22325 = CARTESIAN_POINT ( 'NONE',  ( 0.3574975638436101444, 4.268512490100411279E-17, -3.115157480314960647 ) ) ;
#22326 = ADVANCED_FACE ( 'NONE', ( #5553 ), #3125, .T. ) ;
#22327 = B_SPLINE_CURVE_WITH_KNOTS ( 'NONE', 3,
 ( #12452, #23352, #3976, #1852, #27714, #7935 ),
 .UNSPECIFIED., .F., .F.,
 ( 4, 2, 4 ),
 ( 0.5000000000000000000, 0.7500000000000000000, 1.000000000000000000 ),
 .UNSPECIFIED. ) ;
#22328 = EDGE_CURVE ( 'NONE', #21657, #7534, #186, .T. ) ;
#22329 = VERTEX_POINT ( 'NONE', #22779 ) ;
#22330 = CYLINDRICAL_SURFACE ( 'NONE', #19201, 0.7874015748031496509 ) ;
#22331 = DIRECTION ( 'NONE',  ( 0.000000000000000000, 1.000000000000000000, 0.000000000000000000 ) ) ;
#22332 = CARTESIAN_POINT ( 'NONE',  ( -0.04838950581351151442, 0.1968503937007873850, -3.611194239255213656 ) ) ;
#22333 = ORIENTED_EDGE ( 'NONE', *, *, #6835, .F. ) ;
#22334 = B_SPLINE_CURVE_WITH_KNOTS ( 'NONE', 3,
 ( #24764, #20540, #3283, #7690, #7254, #11776 ),
 .UNSPECIFIED., .F., .F.,
 ( 4, 2, 4 ),
 ( 8.211396612100036608E-14, 0.0007294428068852505231, 0.001458885613688387043 ),
 .UNSPECIFIED. ) ;
#22335 = DIRECTION ( 'NONE',  ( 0.000000000000000000, 0.000000000000000000, -1.000000000000000000 ) ) ;
#22336 = ORIENTED_EDGE ( 'NONE', *, *, #355, .F. ) ;
#22337 = AXIS2_PLACEMENT_3D ( 'NONE', #23081, #6269, #1877 ) ;
#22338 = DIRECTION ( 'NONE',  ( 0.000000000000000000, -1.000000000000000000, 0.000000000000000000 ) ) ;
#22339 = AXIS2_PLACEMENT_3D ( 'NONE', #3836, #21064, #27287 ) ;
#22340 = CARTESIAN_POINT ( 'NONE',  ( 0.7872492035923605025, 0.4002696914127111261, 0.1724953616442082838 ) ) ;
#22341 = CARTESIAN_POINT ( 'NONE',  ( -2.073220866141732523E-16, 0.07874015748031491790, 1.692913385826771533 ) ) ;
#22342 = B_SPLINE_CURVE_WITH_KNOTS ( 'NONE', 3,
 ( #25009, #8074, #5958, #5672, #14293, #22908 ),
 .UNSPECIFIED., .F., .F.,
 ( 4, 2, 4 ),
 ( 1.217380381967464009, 1.219305002860850085, 1.221229623754233939 ),
 .UNSPECIFIED. ) ;
#22343 = ORIENTED_EDGE ( 'NONE', *, *, #27270, .F. ) ;
#22344 = ORIENTED_EDGE ( 'NONE', *, *, #14142, .F. ) ;
#22345 = CARTESIAN_POINT ( 'NONE',  ( -0.1677079028045458664, 0.2904160862623615391, 1.973425196850393970 ) ) ;
#22346 = CARTESIAN_POINT ( 'NONE',  ( -0.5085118447796660446, 0.06699507805605008082, -1.550196850393700920 ) ) ;
#22347 = CIRCLE ( 'NONE', #11995, 0.5322834645669292097 ) ;
#22348 = CARTESIAN_POINT ( 'NONE',  ( -0.5187889641967551313, -0.1190953285357212593, 0.3401574803149606252 ) ) ;
#22350 = EDGE_CURVE ( 'NONE', #17999, #17434, #7199, .T. ) ;
#22349 = CARTESIAN_POINT ( 'NONE',  ( 0.2031943647053979507, -0.4121342552748326060, -1.928289503579156960 ) ) ;
#22351 = CARTESIAN_POINT ( 'NONE',  ( -0.4382482975805212511, 0.3362148458989001609, 0.9399606299212598381 ) ) ;
#22352 = CARTESIAN_POINT ( 'NONE',  ( 0.000000000000000000, 0.000000000000000000, 0.09685039370078740717 ) ) ;
#22353 = DIRECTION ( 'NONE',  ( -0.7660444431189780135, -0.6427876096865392519, 0.000000000000000000 ) ) ;
#22354 = CARTESIAN_POINT ( 'NONE',  ( 0.5385210225480960844, 0.4284847435812472183, 0.1322834645669291320 ) ) ;
#22355 = CARTESIAN_POINT ( 'NONE',  ( -0.2031943647053863211, 0.4121342552748505916, -1.928289503579144748 ) ) ;
#22356 = EDGE_CURVE ( 'NONE', #16402, #25917, #25710, .T. ) ;
#22357 = CARTESIAN_POINT ( 'NONE',  ( 0.2395669291338582696, 2.933848729453403498E-17, -0.4724409448818898127 ) ) ;
#22358 = ADVANCED_FACE ( 'NONE', ( #1838 ), #12045, .T. ) ;
#22359 = AXIS2_PLACEMENT_3D ( 'NONE', #20475, #22452, #14123 ) ;
#22360 = CARTESIAN_POINT ( 'NONE',  ( -0.002755116926490333833, 0.9391221323908144347, -0.1603125978787048322 ) ) ;
#22361 = CARTESIAN_POINT ( 'NONE',  ( -0.05118110236220472370, 0.6299212598425196763, 0.000000000000000000 ) ) ;
#22362 = ( NAMED_UNIT ( * ) SI_UNIT ( $, .STERADIAN. ) SOLID_ANGLE_UNIT ( ) ) ;
#22363 = CARTESIAN_POINT ( 'NONE',  ( -0.5699748819085075358, -0.3282885190152641242, 0.1461456498326136888 ) ) ;
#22364 = CIRCLE ( 'NONE', #25548, 0.6212598425196850238 ) ;
#22365 = ( NAMED_UNIT ( * ) PLANE_ANGLE_UNIT ( ) SI_UNIT ( $, .RADIAN. ) ) ;
#22366 = CARTESIAN_POINT ( 'NONE',  ( 0.3149606299212598381, 0.000000000000000000, 0.000000000000000000 ) ) ;
#22367 = ORIENTED_EDGE ( 'NONE', *, *, #26753, .T. ) ;
#22368 = DIRECTION ( 'NONE',  ( -0.9790454724845842893, -0.2036417511401760472, 2.493892000000000781E-17 ) ) ;
#22369 = VERTEX_POINT ( 'NONE', #4244 ) ;
#22370 = DIRECTION ( 'NONE',  ( 0.000000000000000000, 0.000000000000000000, -1.000000000000000000 ) ) ;
#22371 = VERTEX_POINT ( 'NONE', #21615 ) ;
#22372 = CARTESIAN_POINT ( 'NONE',  ( -0.2268989272875881757, -0.3929158813954942153, -1.934055118110236338 ) ) ;
#22373 = CARTESIAN_POINT ( 'NONE',  ( 0.4149306118455894365, -0.2388850582575479942, 0.08349695147658099670 ) ) ;
#22374 = DIRECTION ( 'NONE',  ( 0.7660444431189780135, 0.6427876096865393629, 0.000000000000000000 ) ) ;
#22375 = DIRECTION ( 'NONE',  ( 0.5000000010362839475, 0.000000000000000000, 0.8660254031861397417 ) ) ;
#22376 = DIRECTION ( 'NONE',  ( 0.000000000000000000, 1.000000000000000000, 0.000000000000000000 ) ) ;
#22377 = DIRECTION ( 'NONE',  ( 0.000000000000000000, -1.000000000000000000, 0.000000000000000000 ) ) ;
#22378 = CARTESIAN_POINT ( 'NONE',  ( -0.5511811023622047445, 1.131889763744194921, -1.386165176156982434E-16 ) ) ;
#22379 = B_SPLINE_CURVE_WITH_KNOTS ( 'NONE', 3,
 ( #25465, #7956, #25170, #5411, #17951, #5114, #18083, #899 ),
 .UNSPECIFIED., .F., .F.,
 ( 4, 2, 2, 4 ),
 ( 0.5000000000000000000, 0.7499999999999997780, 0.8749999999999997780, 1.000000000000000000 ),
 .UNSPECIFIED. ) ;
#22380 = LINE ( 'NONE', #16175, #18614 ) ;
#22381 = CARTESIAN_POINT ( 'NONE',  ( -0.09762295995069900090, 0.3644697409450268766, -3.100567304031763172 ) ) ;
#22382 = CIRCLE ( 'NONE', #9753, 0.8267716535433071723 ) ;
#22383 = CARTESIAN_POINT ( 'NONE',  ( -0.09842519685039370636, -0.07874015748031495954, 0.04546065111729338803 ) ) ;
#22384 = ORIENTED_EDGE ( 'NONE', *, *, #4559, .F. ) ;
#22385 = FACE_OUTER_BOUND ( 'NONE', #5231, .T. ) ;
#22386 = AXIS2_PLACEMENT_3D ( 'NONE', #9923, #6263, #22785 ) ;
#22387 = EDGE_CURVE ( 'NONE', #26154, #3526, #15773, .T. ) ;
#22388 = PRODUCT_CONTEXT ( 'NONE', #9056, 'mechanical' ) ;
#22389 = CARTESIAN_POINT ( 'NONE',  ( -0.6587140841000099778, 0.005767656754076102253, -0.2362204724409449064 ) ) ;
#22390 = ORIENTED_EDGE ( 'NONE', *, *, #6615, .T. ) ;
#22391 = EDGE_LOOP ( 'NONE', ( #12505, #21649, #2509, #11088, #1252, #6832, #14682, #21077, #18610, #13020, #23710, #5872, #11872, #19880 ) ) ;
#22392 = CARTESIAN_POINT ( 'NONE',  ( -0.3338887748335567229, -0.9504046458032088251, -0.8343382454507303203 ) ) ;
#22393 = CYLINDRICAL_SURFACE ( 'NONE', #15582, 0.2952755905264887182 ) ;
#22394 = CARTESIAN_POINT ( 'NONE',  ( 0.5118110236220472231, 0.000000000000000000, 1.766732283464566899 ) ) ;
#22395 = ORIENTED_EDGE ( 'NONE', *, *, #12759, .T. ) ;
#22396 = DIRECTION ( 'NONE',  ( -1.000000000000000000, 0.000000000000000000, 0.000000000000000000 ) ) ;
#22397 = ORIENTED_EDGE ( 'NONE', *, *, #13838, .T. ) ;
#22398 = AXIS2_PLACEMENT_3D ( 'NONE', #16811, #10291, #14575 ) ;
#22399 = CARTESIAN_POINT ( 'NONE',  ( -0.3384212623783161011, 0.1668516812751324463, -3.100567304031758287 ) ) ;
#22400 = AXIS2_PLACEMENT_3D ( 'NONE', #17073, #10559, #6210 ) ;
#22401 = ORIENTED_EDGE ( 'NONE', *, *, #19334, .F. ) ;
#22402 = CARTESIAN_POINT ( 'NONE',  ( -0.6155566689407767633, 1.104160307814390229, -0.07772139087775030430 ) ) ;
#22403 = CARTESIAN_POINT ( 'NONE',  ( -0.4061284506584276199, -0.2351468520616558922, 0.07637795275590551769 ) ) ;
#22404 = ORIENTED_EDGE ( 'NONE', *, *, #1101, .T. ) ;
#22405 = ORIENTED_EDGE ( 'NONE', *, *, #18511, .T. ) ;
#22406 = ORIENTED_EDGE ( 'NONE', *, *, #5893, .T. ) ;
#22407 = ORIENTED_EDGE ( 'NONE', *, *, #10935, .T. ) ;
#22408 = FACE_OUTER_BOUND ( 'NONE', #10207, .T. ) ;
#22409 = VERTEX_POINT ( 'NONE', #9786 ) ;
#22410 = DIRECTION ( 'NONE',  ( 0.000000000000000000, -1.000000000000000000, 0.000000000000000000 ) ) ;
#22411 = VERTEX_POINT ( 'NONE', #18925 ) ;
#22412 = CARTESIAN_POINT ( 'NONE',  ( 0.4218945342797220666, 0.1432577568504696530, -1.934055118110236338 ) ) ;
#22413 = EDGE_CURVE ( 'NONE', #21723, #10388, #23003, .T. ) ;
#22414 = CARTESIAN_POINT ( 'NONE',  ( -0.4921259842519685179, 6.026805113914139867E-17, -1.894685039405410665 ) ) ;
#22415 = CARTESIAN_POINT ( 'NONE',  ( 0.03937007874015747977, 4.580371886574746102E-17, 0.3740157480314960647 ) ) ;
#22416 = EDGE_CURVE ( 'NONE', #17537, #1638, #894, .T. ) ;
#22417 = PRODUCT_DEFINITION ( 'UNKNOWN', '', #7063, #20403 ) ;
#22418 = CARTESIAN_POINT ( 'NONE',  ( -0.03962771305321603071, 0.1968503937007874127, -3.203827438958285256 ) ) ;
#22419 = DIRECTION ( 'NONE',  ( -1.000000000000000000, -1.224646799147353454E-16, 0.000000000000000000 ) ) ;
#22420 = EDGE_CURVE ( 'NONE', #10381, #4492, #8892, .T. ) ;
#22421 = B_SPLINE_CURVE_WITH_KNOTS ( 'NONE', 2,
 ( #21915, #10896, #17655 ),
 .UNSPECIFIED., .F., .F.,
 ( 3, 3 ),
 ( 0.000000000000000000, 1.000000000000000000 ),
 .UNSPECIFIED. ) ;
#22422 = CYLINDRICAL_SURFACE ( 'NONE', #15508, 0.1181102362204720091 ) ;
#22423 = EDGE_CURVE ( 'NONE', #26850, #25174, #827, .T. ) ;
#22424 = CARTESIAN_POINT ( 'NONE',  ( 0.2161381151963047975, 0.2817310484609297228, 1.953740157480315043 ) ) ;
#22425 = CARTESIAN_POINT ( 'NONE',  ( -0.7214243740405492655, -0.1654689342657525153, 0.2562996995995516225 ) ) ;
#22426 = DIRECTION ( 'NONE',  ( 0.000000000000000000, 1.000000000000000000, 0.000000000000000000 ) ) ;
#22427 = DIRECTION ( 'NONE',  ( 0.000000000000000000, 0.000000000000000000, 1.000000000000000000 ) ) ;
#22428 = ( REPRESENTATION_RELATIONSHIP ('NONE','NONE', #12434, #6338 ) REPRESENTATION_RELATIONSHIP_WITH_TRANSFORMATION ( #15814 )SHAPE_REPRESENTATION_RELATIONSHIP( ) ) ;
#22429 = FACE_OUTER_BOUND ( 'NONE', #23306, .T. ) ;
#22430 = CARTESIAN_POINT ( 'NONE',  ( 0.3855916753051596424, -0.3382184156732262470, 1.747047244094488194 ) ) ;
#22431 = CARTESIAN_POINT ( 'NONE',  ( 0.03349795313264332386, 0.5118110236220472231, 1.766732283464566899 ) ) ;
#22432 = CARTESIAN_POINT ( 'NONE',  ( 0.3986320731132086959, -0.2308081338369904478, 0.1771653543307089018 ) ) ;
#22433 = VERTEX_POINT ( 'NONE', #27697 ) ;
#22434 = CARTESIAN_POINT ( 'NONE',  ( 0.000000000000000000, 0.000000000000000000, 0.2362204724409449064 ) ) ;
#22435 = VERTEX_POINT ( 'NONE', #8349 ) ;
#22436 = CIRCLE ( 'NONE', #9344, 0.1082677165354330312 ) ;
#22437 = FACE_OUTER_BOUND ( 'NONE', #4436, .T. ) ;
#22438 = ORIENTED_EDGE ( 'NONE', *, *, #12493, .F. ) ;
#22439 = ORIENTED_EDGE ( 'NONE', *, *, #22642, .F. ) ;
#22440 = CARTESIAN_POINT ( 'NONE',  ( -0.4270824798167633385, 0.2466292688015202517, -1.569881889763779625 ) ) ;
#22441 = ORIENTED_EDGE ( 'NONE', *, *, #20086, .T. ) ;
#22442 = CARTESIAN_POINT ( 'NONE',  ( 0.4382482975805214731, -0.3362148458988676314, 0.9399606299212598381 ) ) ;
#22443 = EDGE_LOOP ( 'NONE', ( #19872, #20034, #7218, #11332 ) ) ;
#22444 = FACE_OUTER_BOUND ( 'NONE', #10216, .T. ) ;
#22445 = ADVANCED_FACE ( 'NONE', ( #19209, #27838 ), #17636, .T. ) ;
#22446 = DIRECTION ( 'NONE',  ( -1.000000000000000000, 0.000000000000000000, 0.000000000000000000 ) ) ;
#22447 = AXIS2_PLACEMENT_3D ( 'NONE', #22506, #11761, #13740 ) ;
#22448 = CARTESIAN_POINT ( 'NONE',  ( 0.1512834625132478961, 0.4870552862735379462, -0.04694520391020851752 ) ) ;
#22449 = EDGE_CURVE ( 'NONE', #22055, #19192, #24141, .T. ) ;
#22450 = CARTESIAN_POINT ( 'NONE',  ( 0.000000000000000000, 0.000000000000000000, -4.330708661396418080 ) ) ;
#22451 = CYLINDRICAL_SURFACE ( 'NONE', #27192, 0.3771653543307086909 ) ;
#22452 = DIRECTION ( 'NONE',  ( -0.000000000000000000, -1.000000000000000000, -0.000000000000000000 ) ) ;
#22453 = EDGE_CURVE ( 'NONE', #15244, #17335, #21650, .T. ) ;
#22454 = CARTESIAN_POINT ( 'NONE',  ( -0.3751294191746886164, 0.2999672986753446069, 0.2362204724409450174 ) ) ;
#22455 = CARTESIAN_POINT ( 'NONE',  ( -0.3988311005573527690, 0.4763376377694653607, 0.2574803149606298969 ) ) ;
#22456 = ADVANCED_FACE ( 'NONE', ( #15412 ), #11143, .F. ) ;
#22457 = CARTESIAN_POINT ( 'NONE',  ( -0.3324885138898230341, 0.04380447413659110945, 1.953740157480315043 ) ) ;
#22458 = CARTESIAN_POINT ( 'NONE',  ( -0.1771653543307086520, 0.8267716535433071723, 0.000000000000000000 ) ) ;
#22459 = CARTESIAN_POINT ( 'NONE',  ( -0.4921259842519685179, 3.013402556957069934E-17, -1.569881889763779625 ) ) ;
#22460 = CARTESIAN_POINT ( 'NONE',  ( -0.1188866373884864824, -0.4438564651657386229, -1.928289503579162067 ) ) ;
#22461 = CARTESIAN_POINT ( 'NONE',  ( 0.4339912984563291110, -0.2498791196563492356, 0.09685039370078740717 ) ) ;
#22462 = AXIS2_PLACEMENT_3D ( 'NONE', #7403, #20545, #16173 ) ;
#22463 = DIRECTION ( 'NONE',  ( -1.000000000000000000, 0.000000000000000000, 0.000000000000000000 ) ) ;
#22464 = PRODUCT_DEFINITION_SHAPE ( 'NONE', 'NONE',  #18243 ) ;
#22465 = DIRECTION ( 'NONE',  ( -0.000000000000000000, -0.000000000000000000, -1.000000000000000000 ) ) ;
#22466 = EDGE_CURVE ( 'NONE', #18057, #18836, #18328, .T. ) ;
#22467 = DIRECTION ( 'NONE',  ( 0.000000000000000000, 0.000000000000000000, 1.000000000000000000 ) ) ;
#22468 = B_SPLINE_CURVE_WITH_KNOTS ( 'NONE', 3,
 ( #19214, #14999, #6650, #23481, #15276, #8353, #4525, #21620 ),
 .UNSPECIFIED., .F., .F.,
 ( 4, 2, 2, 4 ),
 ( 0.5000000000000000000, 0.7500000000000000000, 0.8750000000000001110, 1.000000000000000000 ),
 .UNSPECIFIED. ) ;
#22469 = CARTESIAN_POINT ( 'NONE',  ( -0.1968503937007874127, -1.676732283464567127E-17, -0.09092130223458683158 ) ) ;
#22470 = CARTESIAN_POINT ( 'NONE',  ( -0.03349795313264251895, -0.5118110236220472231, 1.747047244094488194 ) ) ;
#22471 = ORIENTED_EDGE ( 'NONE', *, *, #12510, .T. ) ;
#22472 = DIRECTION ( 'NONE',  ( 0.000000000000000000, 0.000000000000000000, 1.000000000000000000 ) ) ;
#22473 = CARTESIAN_POINT ( 'NONE',  ( 0.3543307086367249448, 0.000000000000000000, -0.1377952755696461029 ) ) ;
#22474 = CARTESIAN_POINT ( 'NONE',  ( -0.02576258753917910760, 0.1968503937008544147, -3.644091798679130800 ) ) ;
#22475 = ORIENTED_EDGE ( 'NONE', *, *, #11319, .F. ) ;
#22476 = DIRECTION ( 'NONE',  ( 0.000000000000000000, 1.000000000000000000, 0.000000000000000000 ) ) ;
#22477 = ORIENTED_EDGE ( 'NONE', *, *, #10981, .T. ) ;
#22478 = CIRCLE ( 'NONE', #7604, 0.1082677165354330728 ) ;
#22479 = EDGE_CURVE ( 'NONE', #17871, #21791, #2479, .T. ) ;
#22480 = LINE ( 'NONE', #20501, #21567 ) ;
#22481 = CIRCLE ( 'NONE', #22020, 0.8163976377952757435 ) ;
#22482 = AXIS2_PLACEMENT_3D ( 'NONE', #11190, #9064, #13313 ) ;
#22483 = DIRECTION ( 'NONE',  ( 0.000000000000000000, 1.224646799147355919E-16, 1.000000000000000000 ) ) ;
#22484 = CARTESIAN_POINT ( 'NONE',  ( 0.7872492035923605025, 0.2525673450849091339, -0.2795801805159861542 ) ) ;
#22485 = EDGE_CURVE ( 'NONE', #11993, #19320, #2782, .T. ) ;
#22486 = B_SPLINE_CURVE_WITH_KNOTS ( 'NONE', 3,
 ( #3599, #18717, #27353, #8005, #1633, #12369, #16607, #25222, #14516, #9919, #3127, #13880, #14027, #26872, #9780, #1445, #18520, #20235 ),
 .UNSPECIFIED., .F., .F.,
 ( 4, 2, 2, 2, 2, 2, 2, 2, 4 ),
 ( 0.000000000000000000, 0.06250000000000004163, 0.1250000000000000555, 0.1875000000000000278, 0.2500000000000000555, 0.3125000000000000555, 0.3750000000000000000, 0.4375000000000000000, 0.5000000000000000000 ),
 .UNSPECIFIED. ) ;
#22487 = DIRECTION ( 'NONE',  ( 0.000000000000000000, 0.000000000000000000, -1.000000000000000000 ) ) ;
#22488 = ORIENTED_EDGE ( 'NONE', *, *, #25443, .F. ) ;
#22489 = CIRCLE ( 'NONE', #5329, 0.8267716535433071723 ) ;
#22490 = CARTESIAN_POINT ( 'NONE',  ( 0.2041304421298337501, 0.2660793235464286033, 1.973425196850393970 ) ) ;
#22491 = CARTESIAN_POINT ( 'NONE',  ( -0.1327036767636164405, 0.4954415918535620134, -1.550196850393700920 ) ) ;
#22492 = CARTESIAN_POINT ( 'NONE',  ( -0.4834654033843718834, -0.1110087727128845347, 0.2989974301282019020 ) ) ;
#22493 = CARTESIAN_POINT ( 'NONE',  ( 0.1775991818008606782, -0.5230301363771325818, 0.9202755905511811330 ) ) ;
#22494 = EDGE_CURVE ( 'NONE', #9880, #16039, #11713, .T. ) ;
#22495 = DIRECTION ( 'NONE',  ( 0.000000000000000000, 1.000000000000000000, 0.000000000000000000 ) ) ;
#22496 = DIRECTION ( 'NONE',  ( 0.000000000000000000, 0.000000000000000000, 1.000000000000000000 ) ) ;
#22497 = CARTESIAN_POINT ( 'NONE',  ( 0.2720459371704843088, 0.3242117229735830830, 0.06102165354330708891 ) ) ;
#22498 = AXIS2_PLACEMENT_3D ( 'NONE', #11963, #7868, #25090 ) ;
#22499 = CARTESIAN_POINT ( 'NONE',  ( 0.03532354024591720376, -0.8267716535433070613, 0.7500000000000001110 ) ) ;
#22500 = ORIENTED_EDGE ( 'NONE', *, *, #12419, .T. ) ;
#22501 = CIRCLE ( 'NONE', #1294, 0.1298643763538141760 ) ;
#22502 = AXIS2_PLACEMENT_3D ( 'NONE', #13520, #22145, #26799 ) ;
#22503 = CARTESIAN_POINT ( 'NONE',  ( -0.2490711204941346568, 1.208528701367826752, -0.6047752023237676910 ) ) ;
#22504 = DIRECTION ( 'NONE',  ( 0.000000000000000000, 1.000000000000000000, 0.000000000000000000 ) ) ;
#22505 = DIRECTION ( 'NONE',  ( 0.000000000000000000, 0.000000000000000000, 1.000000000000000000 ) ) ;
#22506 = CARTESIAN_POINT ( 'NONE',  ( 0.1755067523729419432, 0.3028750839302637998, 0.5245950337139047015 ) ) ;
#22507 = VERTEX_POINT ( 'NONE', #21889 ) ;
#22508 = DIRECTION ( 'NONE',  ( -0.000000000000000000, -0.000000000000000000, 1.000000000000000000 ) ) ;
#22509 = DIRECTION ( 'NONE',  ( -1.000000000000000000, 0.000000000000000000, 0.000000000000000000 ) ) ;
#22510 = EDGE_LOOP ( 'NONE', ( #24968, #27403, #22191, #16899 ) ) ;
#22511 = DIRECTION ( 'NONE',  ( 0.000000000000000000, -1.000000000000000000, 0.000000000000000000 ) ) ;
#22512 = EDGE_LOOP ( 'NONE', ( #7784, #14399 ) ) ;
#22513 = ADVANCED_FACE ( 'NONE', ( #8752 ), #4515, .T. ) ;
#22514 = CARTESIAN_POINT ( 'NONE',  ( -0.4069519308876702324, -0.2006393256663696334, -1.934055118110236338 ) ) ;
#22515 = CYLINDRICAL_SURFACE ( 'NONE', #27034, 1.131889763779527547 ) ;
#22516 = CARTESIAN_POINT ( 'NONE',  ( -0.2720459371704843088, 0.3242117229735834716, 0.1377952755905511861 ) ) ;
#22517 = CARTESIAN_POINT ( 'NONE',  ( -0.006547182368340512953, 0.3149607547026831433, -3.174212199124641920 ) ) ;
#22518 = CARTESIAN_POINT ( 'NONE',  ( -0.4681308612729627172, -0.1074986424507606841, 0.2362204724409447676 ) ) ;
#22519 = EDGE_LOOP ( 'NONE', ( #12015, #24800, #6810, #7389 ) ) ;
#22520 = FACE_BOUND ( 'NONE', #8304, .T. ) ;
#22521 = EDGE_CURVE ( 'NONE', #23339, #280, #6002, .T. ) ;
#22522 = ORIENTED_EDGE ( 'NONE', *, *, #11034, .T. ) ;
#22523 = LINE ( 'NONE', #9938, #26984 ) ;
#22524 = CIRCLE ( 'NONE', #25678, 0.1308464566929133932 ) ;
#22525 = CARTESIAN_POINT ( 'NONE',  ( -0.2158067241047623985, -0.4466421405382755561, 0.1734435147819099465 ) ) ;
#22526 = ORIENTED_EDGE ( 'NONE', *, *, #12071, .F. ) ;
#22527 = CARTESIAN_POINT ( 'NONE',  ( -0.1668516812751398570, -0.3384212623783108276, -3.100567304031765392 ) ) ;
#22528 = AXIS2_PLACEMENT_3D ( 'NONE', #23139, #3619, #10259 ) ;
#22529 = DIRECTION ( 'NONE',  ( 0.000000000000000000, 0.000000000000000000, 1.000000000000000000 ) ) ;
#22530 = ORIENTED_EDGE ( 'NONE', *, *, #18612, .T. ) ;
#22531 = CARTESIAN_POINT ( 'NONE',  ( -0.3929158813954827245, 0.2268989272876178465, -1.934055118110236338 ) ) ;
#22532 = AXIS2_PLACEMENT_3D ( 'NONE', #1159, #17930, #22338 ) ;
#22533 = EDGE_CURVE ( 'NONE', #19192, #24677, #20866, .T. ) ;
#22534 = ORIENTED_EDGE ( 'NONE', *, *, #12766, .T. ) ;
#22535 = CARTESIAN_POINT ( 'NONE',  ( -0.3861436020174326966, -0.6370004219456083527, -0.5391745765651102529 ) ) ;
#22536 = CARTESIAN_POINT ( 'NONE',  ( -0.6102362204724409711, 1.112204724409448842, -1.362057955744595713E-16 ) ) ;
#22537 = CARTESIAN_POINT ( 'NONE',  ( 0.4856708409200598542, 0.1649135259617023896, 1.747047244094488194 ) ) ;
#22538 = LENGTH_MEASURE_WITH_UNIT ( LENGTH_MEASURE( 0.02539999999999999897 ), #3018 ) ;
#22539 = ORIENTED_EDGE ( 'NONE', *, *, #3464, .F. ) ;
#22540 = CIRCLE ( 'NONE', #10359, 0.1003937007874015908 ) ;
#22541 = CARTESIAN_POINT ( 'NONE',  ( -0.3572819248074403653, -0.1213180142433946673, -3.100567304031765392 ) ) ;
#22542 = ORIENTED_EDGE ( 'NONE', *, *, #20277, .T. ) ;
#22543 = CARTESIAN_POINT ( 'NONE',  ( 0.000000000000000000, 0.000000000000000000, 0.1377952755905511861 ) ) ;
#22544 = AXIS2_PLACEMENT_3D ( 'NONE', #13264, #8883, #177 ) ;
#22545 = LINE ( 'NONE', #12224, #18102 ) ;
#22546 = EDGE_LOOP ( 'NONE', ( #3914, #6008, #6436, #23185, #12503, #563 ) ) ;
#22547 = ORIENTED_EDGE ( 'NONE', *, *, #13471, .T. ) ;
#22548 = CARTESIAN_POINT ( 'NONE',  ( 0.6299212598425196763, 4.580371886574746102E-17, 0.3740157480314960647 ) ) ;
#22549 = ORIENTED_EDGE ( 'NONE', *, *, #3742, .T. ) ;
#22550 = CARTESIAN_POINT ( 'NONE',  ( -0.02909913904662089768, -0.4446020952038907681, -1.934055118110236338 ) ) ;
#22551 = VERTEX_POINT ( 'NONE', #26386 ) ;
#22552 = DIRECTION ( 'NONE',  ( -0.000000000000000000, -0.000000000000000000, -1.000000000000000000 ) ) ;
#22553 = CARTESIAN_POINT ( 'NONE',  ( 0.000000000000000000, 0.6102362204724409711, 0.4724409448818898127 ) ) ;
#22554 = EDGE_CURVE ( 'NONE', #26747, #16795, #1030, .T. ) ;
#22555 = CARTESIAN_POINT ( 'NONE',  ( -0.1786951194748074845, 0.8740064756424290593, -0.6084677936387519193 ) ) ;
#22556 = CARTESIAN_POINT ( 'NONE',  ( 0.2395669291338582696, 2.933848729453403498E-17, -0.02362204724409448786 ) ) ;
#22557 = CARTESIAN_POINT ( 'NONE',  ( -0.3259357382551450466, 0.08759279594700321303, 1.973425196850394192 ) ) ;
#22558 = CARTESIAN_POINT ( 'NONE',  ( -0.3040421205569480145, 0.9438032647596121816, -0.7968182652463602356 ) ) ;
#22559 = AXIS2_PLACEMENT_3D ( 'NONE', #3896, #23549, #12516 ) ;
#22560 = AXIS2_PLACEMENT_3D ( 'NONE', #21736, #4498, #13379 ) ;
#22561 = DIRECTION ( 'NONE',  ( 0.000000000000000000, 0.000000000000000000, 1.000000000000000000 ) ) ;
#22562 = CARTESIAN_POINT ( 'NONE',  ( 0.000000000000000000, 0.3543307086614172485, 0.000000000000000000 ) ) ;
#22563 = CARTESIAN_POINT ( 'NONE',  ( 0.6119360453657125554, 0.1072290460171897442, 0.09685039370078740717 ) ) ;
#22564 = CARTESIAN_POINT ( 'NONE',  ( -0.04638120790932972332, -0.3520466617656973218, 1.953740157480315043 ) ) ;
#22565 = ORIENTED_EDGE ( 'NONE', *, *, #5552, .F. ) ;
#22566 = CARTESIAN_POINT ( 'NONE',  ( -0.6707652279343464530, -0.1538768215239710857, 0.1322834645669291320 ) ) ;
#22567 = CARTESIAN_POINT ( 'NONE',  ( -0.4535326485287285991, 0.08054850140359781641, 0.1639447408838820286 ) ) ;
#22568 = CARTESIAN_POINT ( 'NONE',  ( 0.000000000000000000, 0.3937007873309092409, 0.000000000000000000 ) ) ;
#22569 = CARTESIAN_POINT ( 'NONE',  ( 0.000000000000000000, 0.000000000000000000, 0.06614173228346456601 ) ) ;
#22570 = CARTESIAN_POINT ( 'NONE',  ( 0.1712563538833041243, 0.5043504886477225835, 1.747047244094488194 ) ) ;
#22571 = CARTESIAN_POINT ( 'NONE',  ( 0.3855916753051394363, 0.3382184156732163660, 1.766732283464566899 ) ) ;
#22572 = EDGE_CURVE ( 'NONE', #3499, #17056, #26742, .T. ) ;
#22573 = B_SPLINE_CURVE_WITH_KNOTS ( 'NONE', 3,
 ( #20704, #27068, #11520, #7283 ),
 .UNSPECIFIED., .F., .F.,
 ( 4, 4 ),
 ( -1.199999999999999956, -0.5999999999999999778 ),
 .UNSPECIFIED. ) ;
#22574 = ORIENTED_EDGE ( 'NONE', *, *, #7388, .F. ) ;
#22575 = CARTESIAN_POINT ( 'NONE',  ( 0.1490609433615240342, 0.4786070381542913421, 0.000000000000000000 ) ) ;
#22576 = VERTEX_POINT ( 'NONE', #4916 ) ;
#22577 = CARTESIAN_POINT ( 'NONE',  ( 0.4092566936336781147, 0.3255244810065535677, 0.1392975274217217729 ) ) ;
#22578 = CARTESIAN_POINT ( 'NONE',  ( -0.2647715730835492609, -0.5498038367121063086, 0.3661437007874016047 ) ) ;
#22579 = CARTESIAN_POINT ( 'NONE',  ( -0.2938049579018706114, 0.3349573549949406148, -1.934055118110236338 ) ) ;
#22580 = DIRECTION ( 'NONE',  ( 0.000000000000000000, 0.000000000000000000, -1.000000000000000000 ) ) ;
#22581 = ORIENTED_EDGE ( 'NONE', *, *, #14071, .F. ) ;
#22582 = CARTESIAN_POINT ( 'NONE',  ( 0.3169330146514671709, -0.1835719822061527007, 0.08455817587548536407 ) ) ;
#22583 = ORIENTED_EDGE ( 'NONE', *, *, #14827, .T. ) ;
#22584 = ORIENTED_EDGE ( 'NONE', *, *, #16975, .T. ) ;
#22585 = CARTESIAN_POINT ( 'NONE',  ( -0.1275996891957733581, -0.4763861460130334735, -1.569881889763779625 ) ) ;
#22586 = ADVANCED_FACE ( 'NONE', ( #688 ), #9016, .T. ) ;
#22587 = ORIENTED_EDGE ( 'NONE', *, *, #13152, .T. ) ;
#22588 = ORIENTED_EDGE ( 'NONE', *, *, #8388, .T. ) ;
#22589 = ITEM_DEFINED_TRANSFORMATION ( 'NONE', 'NONE', #8908,  #11588 ) ;
#22590 = DIRECTION ( 'NONE',  ( -0.000000000000000000, 0.8660254037844388186, 0.4999999999999998890 ) ) ;
#22591 = CARTESIAN_POINT ( 'NONE',  ( -0.1634143070178008805, -0.4472844159266942121, 0.2330651858521301523 ) ) ;
#22592 = CARTESIAN_POINT ( 'NONE',  ( 0.5381367953593070297, -0.3104394140547551140, 0.09684793308443542803 ) ) ;
#22593 = DIRECTION ( 'NONE',  ( 0.000000000000000000, 0.000000000000000000, 1.000000000000000000 ) ) ;
#22594 = DIRECTION ( 'NONE',  ( 0.6427876096865399180, 0.7660444431189776804, -0.000000000000000000 ) ) ;
#22595 = APPLICATION_CONTEXT ( 'automotive_design' ) ;
#22596 = UNCERTAINTY_MEASURE_WITH_UNIT (LENGTH_MEASURE( 1.000000000000000082E-05 ), #15709, 'distance_accuracy_value', 'NONE') ;
#22597 = ORIENTED_EDGE ( 'NONE', *, *, #3325, .F. ) ;
#22598 = DIRECTION ( 'NONE',  ( 1.000000000000000000, 0.000000000000000000, 0.000000000000000000 ) ) ;
#22599 = FACE_OUTER_BOUND ( 'NONE', #20396, .T. ) ;
#22600 = CARTESIAN_POINT ( 'NONE',  ( -1.357510822077637958, -1.563633646945708833, 2.145669291338582862 ) ) ;
#22601 = EDGE_CURVE ( 'NONE', #24837, #5489, #16870, .T. ) ;
#22602 = TOROIDAL_SURFACE ( 'NONE', #24854, 0.4232283464566928832, 0.07677165354330708902 ) ;
#22603 = DIRECTION ( 'NONE',  ( 0.000000000000000000, 0.000000000000000000, 1.000000000000000000 ) ) ;
#22604 = DIRECTION ( 'NONE',  ( 0.000000000000000000, 1.000000000000000000, 0.000000000000000000 ) ) ;
#22605 = CYLINDRICAL_SURFACE ( 'NONE', #9668, 1.377952755905512472 ) ;
#22606 = EDGE_CURVE ( 'NONE', #14790, #18347, #15540, .T. ) ;
#22607 = CARTESIAN_POINT ( 'NONE',  ( -0.2997912780622380979, -0.1736589463928937815, 0.1377952755905510751 ) ) ;
#22608 = CIRCLE ( 'NONE', #27134, 0.6212598425196850238 ) ;
#22609 = AXIS2_PLACEMENT_3D ( 'NONE', #4733, #17598, #515 ) ;
#22610 = ORIENTED_EDGE ( 'NONE', *, *, #26022, .F. ) ;
#22611 = VERTEX_POINT ( 'NONE', #18022 ) ;
#22612 = EDGE_CURVE ( 'NONE', #16929, #8378, #25765, .T. ) ;
#22613 = ORIENTED_EDGE ( 'NONE', *, *, #1096, .T. ) ;
#22614 = DIRECTION ( 'NONE',  ( 1.000000000000000000, 0.000000000000000000, 0.000000000000000000 ) ) ;
#22615 = ADVANCED_FACE ( 'NONE', ( #27243 ), #21817, .T. ) ;
#22616 = FACE_OUTER_BOUND ( 'NONE', #7083, .T. ) ;
#22617 = CARTESIAN_POINT ( 'NONE',  ( 0.09842519684999338769, 0.1968503937007873850, -3.561114497143033297 ) ) ;
#22618 = EDGE_LOOP ( 'NONE', ( #357, #11551, #24378, #17320, #23253, #1821, #10808, #16268, #12821, #1897, #9856 ) ) ;
#22619 = CARTESIAN_POINT ( 'NONE',  ( -0.3430989538740937816, 0.06100393589341226996, 0.1589462317956309712 ) ) ;
#22620 = ORIENTED_EDGE ( 'NONE', *, *, #10189, .T. ) ;
#22621 = CARTESIAN_POINT ( 'NONE',  ( -0.3149606299212598381, 3.857155272905049219E-17, -3.115157480314960647 ) ) ;
#22622 = VECTOR ( 'NONE', #3561, 39.37007874015748143 ) ;
#22623 = CARTESIAN_POINT ( 'NONE',  ( 0.7845931698711713365, 0.3299597629270051846, -0.3067722674759077450 ) ) ;
#22624 = CIRCLE ( 'NONE', #24874, 0.4606299212598425341 ) ;
#22625 = CARTESIAN_POINT ( 'NONE',  ( 0.3667122560601320802, 0.09855118063547671503, -3.100567304031762728 ) ) ;
#22626 = DIRECTION ( 'NONE',  ( 1.000000000000000000, 0.000000000000000000, 0.000000000000000000 ) ) ;
#22627 = DIRECTION ( 'NONE',  ( 0.000000000000000000, 0.000000000000000000, 1.000000000000000000 ) ) ;
#22628 = ORIENTED_EDGE ( 'NONE', *, *, #17874, .T. ) ;
#22629 = CARTESIAN_POINT ( 'NONE',  ( -0.08676778863011327947, 0.3239425792934402248, 1.973425196850393970 ) ) ;
#22630 = CARTESIAN_POINT ( 'NONE',  ( -0.03349795313024159921, 0.5118110236220473341, -1.550196850393700920 ) ) ;
#22631 = CARTESIAN_POINT ( 'NONE',  ( 0.000000000000000000, 0.000000000000000000, 0.07637795275590551769 ) ) ;
#22632 = CARTESIAN_POINT ( 'NONE',  ( -0.2442565704126240245, -0.4954197419817664150, 0.9202755905511811330 ) ) ;
#22633 = CARTESIAN_POINT ( 'NONE',  ( 0.000000000000000000, 0.4724409448818898127, -2.066929133858267598 ) ) ;
#22634 = DIRECTION ( 'NONE',  ( 0.000000000000000000, 0.000000000000000000, 1.000000000000000000 ) ) ;
#22635 = ORIENTED_EDGE ( 'NONE', *, *, #3500, .F. ) ;
#22636 = CARTESIAN_POINT ( 'NONE',  ( 0.000000000000000000, 0.000000000000000000, 0.01181102362204724393 ) ) ;
#22637 = ADVANCED_FACE ( 'NONE', ( #7319 ), #7828, .F. ) ;
#22638 = FACE_BOUND ( 'NONE', #1482, .T. ) ;
#22639 = VECTOR ( 'NONE', #13000, 39.37007874015748143 ) ;
#22640 = LINE ( 'NONE', #18375, #10161 ) ;
#22641 = CARTESIAN_POINT ( 'NONE',  ( 1.692913385826771533, 0.07874015748031491790, -0.1181102362204716899 ) ) ;
#22642 = EDGE_CURVE ( 'NONE', #9472, #24177, #7905, .T. ) ;
#22643 = CARTESIAN_POINT ( 'NONE',  ( 0.3217486617182078734, 0.3837523410419874659, 0.2574827755769819038 ) ) ;
#22644 = ORIENTED_EDGE ( 'NONE', *, *, #24883, .F. ) ;
#22645 = AXIS2_PLACEMENT_3D ( 'NONE', #4702, #11759, #26726 ) ;
#22646 = DIRECTION ( 'NONE',  ( 0.000000000000000000, -1.000000000000000000, 0.000000000000000000 ) ) ;
#22647 = DIRECTION ( 'NONE',  ( 0.8660254037844385966, -0.5000000000000003331, 0.000000000000000000 ) ) ;
#22648 = CARTESIAN_POINT ( 'NONE',  ( -0.6119360453657125554, 0.1072290460171901605, 0.09685039370078740717 ) ) ;
#22649 = ORIENTED_EDGE ( 'NONE', *, *, #8862, .F. ) ;
#22650 = CARTESIAN_POINT ( 'NONE',  ( -0.3543307086614173596, 4.268512490100411279E-17, 1.953740157480315043 ) ) ;
#22651 = VERTEX_POINT ( 'NONE', #20315 ) ;
#22652 = CARTESIAN_POINT ( 'NONE',  ( 0.1173917140416396443, 0.4382752542996237732, -1.934055118110236338 ) ) ;
#22653 = CARTESIAN_POINT ( 'NONE',  ( -0.3937007874015748254, 0.000000000000000000, 0.000000000000000000 ) ) ;
#22654 = DIRECTION ( 'NONE',  ( -0.000000000000000000, -1.000000000000000000, -0.000000000000000000 ) ) ;
#22655 = FACE_OUTER_BOUND ( 'NONE', #23564, .T. ) ;
#22656 = FACE_OUTER_BOUND ( 'NONE', #2331, .T. ) ;
#22657 = ORIENTED_EDGE ( 'NONE', *, *, #20245, .F. ) ;
#22658 = LINE ( 'NONE', #7971, #951 ) ;
#22659 = VERTEX_POINT ( 'NONE', #22578 ) ;
#22660 = CIRCLE ( 'NONE', #10475, 0.05216535433070866590 ) ;
#22661 = ADVANCED_FACE ( 'NONE', ( #25114 ), #24969, .F. ) ;
#22662 = CARTESIAN_POINT ( 'NONE',  ( 0.1755067523729419432, 0.3028750839302634112, -0.5245950337139054787 ) ) ;
#22663 = DIRECTION ( 'NONE',  ( 0.000000000000000000, 0.000000000000000000, 1.000000000000000000 ) ) ;
#22664 = ORIENTED_EDGE ( 'NONE', *, *, #13600, .T. ) ;
#22665 = CARTESIAN_POINT ( 'NONE',  ( -0.3267488823401750730, -0.1886891683788910756, -3.100567304031762284 ) ) ;
#22666 = ( LENGTH_UNIT ( ) NAMED_UNIT ( * ) SI_UNIT ( $, .METRE. ) ) ;
#22667 = EDGE_LOOP ( 'NONE', ( #10227, #15366, #3451, #12939 ) ) ;
#22668 = CARTESIAN_POINT ( 'NONE',  ( -0.4303822302053990634, -0.1152775731717099322, -1.934055118110236338 ) ) ;
#22670 = VECTOR ( 'NONE', #16958, 39.37007874015748143 ) ;
#22669 = CARTESIAN_POINT ( 'NONE',  ( 0.4121342552748534227, 0.2031943647053804092, -1.928289503579144304 ) ) ;
#22671 = ORIENTED_EDGE ( 'NONE', *, *, #23404, .F. ) ;
#22672 = B_SPLINE_CURVE_WITH_KNOTS ( 'NONE', 2,
 ( #12128, #18899, #27398 ),
 .UNSPECIFIED., .F., .F.,
 ( 3, 3 ),
 ( 0.000000000000000000, 1.000000000000000000 ),
 .UNSPECIFIED. ) ;
#22673 = CARTESIAN_POINT ( 'NONE',  ( -0.4280150452258433269, -0.7349289522583307699, -0.1909859530666125904 ) ) ;
#22674 = CARTESIAN_POINT ( 'NONE',  ( 0.1516263115863346334, 0.2937912646890007973, 0.3972688187320929099 ) ) ;
#22675 = CARTESIAN_POINT ( 'NONE',  ( 0.1327036767659768302, -0.4954415918531079877, 1.747047244094488194 ) ) ;
#22676 = EDGE_CURVE ( 'NONE', #4895, #12340, #11424, .T. ) ;
#22677 = ORIENTED_EDGE ( 'NONE', *, *, #5327, .F. ) ;
#22678 = AXIS2_PLACEMENT_3D ( 'NONE', #19432, #2196, #9094 ) ;
#22679 = CARTESIAN_POINT ( 'NONE',  ( 0.04928467685643989765, -0.3740848232703748444, -3.100567304031760507 ) ) ;
#22680 = VERTEX_POINT ( 'NONE', #2924 ) ;
#22681 = CARTESIAN_POINT ( 'NONE',  ( -0.6003938747882047178, 1.122047070076019004, -0.01921884795888584296 ) ) ;
#22682 = CARTESIAN_POINT ( 'NONE',  ( -0.08294224740493445769, -0.2841094280683381657, -0.1049447807868563037 ) ) ;
#22683 = EDGE_CURVE ( 'NONE', #18475, #7018, #24540, .T. ) ;
#22684 = ORIENTED_EDGE ( 'NONE', *, *, #27335, .F. ) ;
#22685 = CIRCLE ( 'NONE', #14593, 0.3831516066089791228 ) ;
#22686 = DIRECTION ( 'NONE',  ( -1.000000000000000000, 0.000000000000000000, 0.000000000000000000 ) ) ;
#22687 = DIRECTION ( 'NONE',  ( 0.000000000000000000, 0.000000000000000000, 1.000000000000000000 ) ) ;
#22688 = ORIENTED_EDGE ( 'NONE', *, *, #24229, .F. ) ;
#22689 = VERTEX_POINT ( 'NONE', #18601 ) ;
#22690 = VERTEX_POINT ( 'NONE', #3488 ) ;
#22691 = VERTEX_POINT ( 'NONE', #11984 ) ;
#22692 = PLANE ( 'NONE',  #18163 ) ;
#22693 = EDGE_CURVE ( 'NONE', #18758, #4773, #11553, .T. ) ;
#22694 = CARTESIAN_POINT ( 'NONE',  ( -0.1584254766472275311, 0.3213305936751604253, -3.115157480314960647 ) ) ;
#22695 = DIRECTION ( 'NONE',  ( 1.000000000000000000, 0.000000000000000000, 0.000000000000000000 ) ) ;
#22696 = DIRECTION ( 'NONE',  ( 0.000000000000000000, 0.000000000000000000, 1.000000000000000000 ) ) ;
#22697 = DIRECTION ( 'NONE',  ( -0.2036417511401758251, 0.9790454724845842893, -1.198984999999999602E-16 ) ) ;
#22698 = DIRECTION ( 'NONE',  ( -1.000000000000000000, 0.000000000000000000, 0.000000000000000000 ) ) ;
#22699 = AXIS2_PLACEMENT_3D ( 'NONE', #19563, #245, #4036 ) ;
#22700 = AXIS2_PLACEMENT_3D ( 'NONE', #23200, #16538, #14450 ) ;
#22701 = CARTESIAN_POINT ( 'NONE',  ( -0.4055118110236220486, 4.966087413865251393E-17, 0.01181102362204724393 ) ) ;
#22702 = CARTESIAN_POINT ( 'NONE',  ( 0.5190368482393039606, -0.1180105360553401483, 0.3401591244667909186 ) ) ;
#22703 = CARTESIAN_POINT ( 'NONE',  ( 0.5379168165870354956, -0.3108204284649153659, 0.2574827755769819038 ) ) ;
#22704 = AXIS2_PLACEMENT_3D ( 'NONE', #3632, #12258, #3928 ) ;
#22705 = VERTEX_POINT ( 'NONE', #18316 ) ;
#22706 = CARTESIAN_POINT ( 'NONE',  ( 0.3680051700917441604, 0.000000000000000000, 0.000000000000000000 ) ) ;
#22707 = CARTESIAN_POINT ( 'NONE',  ( -0.09842519685039370636, -1.570035826771653483E-17, -0.09092130223458683158 ) ) ;
#22708 = CARTESIAN_POINT ( 'NONE',  ( 0.4724409448465559103, 6.026805113697782438E-17, 1.953740157480315043 ) ) ;
#22709 = AXIS2_PLACEMENT_3D ( 'NONE', #22562, #5326, #20020 ) ;
#22710 = DIRECTION ( 'NONE',  ( 0.000000000000000000, -1.000000000000000000, 0.000000000000000000 ) ) ;
#22711 = CARTESIAN_POINT ( 'NONE',  ( 0.4856708409200665155, -0.1649135259616916482, 1.747047244094488194 ) ) ;
#22712 = ADVANCED_FACE ( 'NONE', ( #11838 ), #6485, .F. ) ;
#22713 = CARTESIAN_POINT ( 'NONE',  ( 0.06699507805369034341, 0.5085118447801111330, 1.747047244094488194 ) ) ;
#22714 = EDGE_CURVE ( 'NONE', #2281, #2854, #18632, .T. ) ;
#22715 = CARTESIAN_POINT ( 'NONE',  ( 0.1285103288269283661, -0.3545966721392122545, 0.1992125984251968684 ) ) ;
#22716 = ORIENTED_EDGE ( 'NONE', *, *, #9735, .F. ) ;
#22717 = CARTESIAN_POINT ( 'NONE',  ( -0.0005189969344232283309, 0.3771649972486724733, 0.1992125984251968684 ) ) ;
#22718 = DIRECTION ( 'NONE',  ( -0.8571673003991031603, 1.049727190767539389E-16, 0.5150380754143460971 ) ) ;
#22719 = CARTESIAN_POINT ( 'NONE',  ( -0.7874015748031496509, -3.035194737559055338E-06, -1.475314960619023674 ) ) ;
#22720 = EDGE_LOOP ( 'NONE', ( #1664, #12952 ) ) ;
#22721 = ORIENTED_EDGE ( 'NONE', *, *, #14932, .F. ) ;
#22722 = CARTESIAN_POINT ( 'NONE',  ( -0.2466292688015201129, 0.4270824798167635050, -1.569881889763779625 ) ) ;
#22723 = VERTEX_POINT ( 'NONE', #16086 ) ;
#22724 = ORIENTED_EDGE ( 'NONE', *, *, #9281, .T. ) ;
#22725 = AXIS2_PLACEMENT_3D ( 'NONE', #1965, #27260, #10574 ) ;
#22726 = CARTESIAN_POINT ( 'NONE',  ( 0.4930758245789425009, 0.08754571829529310401, 0.2574803149606298969 ) ) ;
#22727 = CIRCLE ( 'NONE', #11019, 0.1181102362204718703 ) ;
#22728 = LINE ( 'NONE', #13986, #824 ) ;
#22729 = CARTESIAN_POINT ( 'NONE',  ( 0.5925575908939920700, 0.000000000000000000, 0.000000000000000000 ) ) ;
#22730 = B_SPLINE_CURVE_WITH_KNOTS ( 'NONE', 3,
 ( #17423, #13323, #8671, #2303, #26315, #8808, #10793, #10931, #19412, #15340 ),
 .UNSPECIFIED., .F., .F.,
 ( 4, 2, 2, 2, 4 ),
 ( 0.000000000000000000, 0.2500000000000000000, 0.5000000000000000000, 0.7500000000000000000, 1.000000000000000000 ),
 .UNSPECIFIED. ) ;
#22731 = EDGE_CURVE ( 'NONE', #13825, #14265, #9575, .T. ) ;
#22732 = ORIENTED_EDGE ( 'NONE', *, *, #24700, .T. ) ;
#22733 = CARTESIAN_POINT ( 'NONE',  ( -0.6707652279343347956, -0.1538768215240151616, 0.3401574803149606252 ) ) ;
#22734 = CARTESIAN_POINT ( 'NONE',  ( 0.1482986320106562672, -0.3007905576423960392, 1.953740157480315043 ) ) ;
#22735 = CIRCLE ( 'NONE', #25446, 0.5007874015748031704 ) ;
#22736 = VERTEX_POINT ( 'NONE', #22717 ) ;
#22737 = SHAPE_REPRESENTATION ( 'Tapered Roller Bearing 17x40x17', ( #11588, #27945, #27969 ), #3496 ) ;
#22738 = FACE_OUTER_BOUND ( 'NONE', #23269, .T. ) ;
#22739 = CARTESIAN_POINT ( 'NONE',  ( -0.3020979083623086536, 0.3591256245825952265, 0.1992125984251968684 ) ) ;
#22740 = DIRECTION ( 'NONE',  ( 1.000000000000000078E-15, -1.000000000000000000, 0.000000000000000000 ) ) ;
#22741 = CARTESIAN_POINT ( 'NONE',  ( -0.3543307086614173596, 4.268512490100411279E-17, 1.953740157480315043 ) ) ;
#22742 = CARTESIAN_POINT ( 'NONE',  ( -0.4300129863948118358, 0.2478439864030018147, -1.569881889763779625 ) ) ;
#22743 = DIRECTION ( 'NONE',  ( 1.000000000000000000, 0.000000000000000000, 0.000000000000000000 ) ) ;
#22744 = TOROIDAL_SURFACE ( 'NONE', #7392, 0.3070866141732283561, 0.01181102362204724393 ) ;
#22745 = ORIENTED_EDGE ( 'NONE', *, *, #8273, .F. ) ;
#22746 = ORIENTED_EDGE ( 'NONE', *, *, #27831, .T. ) ;
#22747 = ( LENGTH_UNIT ( ) NAMED_UNIT ( * ) SI_UNIT ( $, .METRE. ) ) ;
#22748 = VERTEX_POINT ( 'NONE', #3344 ) ;
#22749 = CARTESIAN_POINT ( 'NONE',  ( -9.069736220472442904E-16, -0.8267716535433071723, 0.000000000000000000 ) ) ;
#22750 = LINE ( 'NONE', #27275, #4871 ) ;
#22751 = CARTESIAN_POINT ( 'NONE',  ( 0.6397637795275591399, 0.7874015748031496509, 0.000000000000000000 ) ) ;
#22752 = ORIENTED_EDGE ( 'NONE', *, *, #25747, .F. ) ;
#22753 = CIRCLE ( 'NONE', #8335, 1.377952755905512472 ) ;
#22754 = ORIENTED_EDGE ( 'NONE', *, *, #20927, .F. ) ;
#22755 = SURFACE_STYLE_USAGE ( .BOTH. , #14154 ) ;
#22756 = CARTESIAN_POINT ( 'NONE',  ( -0.2089723435111590921, -0.4324731448915377641, 0.2362204724409450174 ) ) ;
#22757 = EDGE_CURVE ( 'NONE', #18491, #26373, #13951, .T. ) ;
#22758 = EDGE_CURVE ( 'NONE', #24304, #11701, #500, .T. ) ;
#22759 = CIRCLE ( 'NONE', #26367, 0.02362204724409448092 ) ;
#22760 = FACE_OUTER_BOUND ( 'NONE', #24755, .T. ) ;
#22761 = LINE ( 'NONE', #20646, #19659 ) ;
#22762 = CARTESIAN_POINT ( 'NONE',  ( 0.5118096047255313863, -0.03359157810808697381, -1.550196850393700920 ) ) ;
#22763 = ORIENTED_EDGE ( 'NONE', *, *, #2812, .T. ) ;
#22764 = CARTESIAN_POINT ( 'NONE',  ( -0.3007905576423877680, -0.1482986320106428613, 1.973425196850393970 ) ) ;
#22765 = CARTESIAN_POINT ( 'NONE',  ( -0.4932136069632142017, 0.08676634416062008193, 0.2574827755769819038 ) ) ;
#22766 = CARTESIAN_POINT ( 'NONE',  ( 0.5118110236220473341, 0.03349795313024165472, -1.550196850393700920 ) ) ;
#22767 = ADVANCED_FACE ( 'NONE', ( #19031, #1943 ), #25541, .T. ) ;
#22768 = CARTESIAN_POINT ( 'NONE',  ( 0.07214943758244279914, 0.5511811023622046335, 0.9202755905511812440 ) ) ;
#22769 = CARTESIAN_POINT ( 'NONE',  ( -0.2762247810519161129, -0.4783323773986413729, 0.9202755905511811330 ) ) ;
#22770 = CARTESIAN_POINT ( 'NONE',  ( 0.000000000000000000, 0.000000000000000000, 0.1377952755905511861 ) ) ;
#22771 = ADVANCED_FACE ( 'NONE', ( #18 ), #9159, .T. ) ;
#22772 = LINE ( 'NONE', #5543, #19584 ) ;
#22773 = ORIENTED_EDGE ( 'NONE', *, *, #27188, .F. ) ;
#22774 = LINE ( 'NONE', #9776, #26344 ) ;
#22775 = TOROIDAL_SURFACE ( 'NONE', #9223, 0.4986013261500205074, 0.02755905511811023584 ) ;
#22776 = DIRECTION ( 'NONE',  ( 1.000000000000000000, 0.000000000000000000, 0.000000000000000000 ) ) ;
#22777 = CARTESIAN_POINT ( 'NONE',  ( 1.197070535079588716, 0.07874015748031495954, 1.315180771300060503 ) ) ;
#22778 = B_SPLINE_CURVE_WITH_KNOTS ( 'NONE', 3,
 ( #23626, #27859, #2400, #8495, #4262, #15429 ),
 .UNSPECIFIED., .F., .F.,
 ( 4, 2, 4 ),
 ( 0.4045103800603450095, 0.4064350009536160102, 0.4083596218468860117 ),
 .UNSPECIFIED. ) ;
#22779 = CARTESIAN_POINT ( 'NONE',  ( 0.1516263115863346334, 0.2937912646890004087, -0.3972688187320929099 ) ) ;
#22780 = ORIENTED_EDGE ( 'NONE', *, *, #22846, .F. ) ;
#22781 = ORIENTED_EDGE ( 'NONE', *, *, #13412, .T. ) ;
#22782 = CIRCLE ( 'NONE', #12865, 0.3346456692913385988 ) ;
#22783 = CARTESIAN_POINT ( 'NONE',  ( 0.8558003517949211991, 0.6468501409757874132, 1.633858267716535639 ) ) ;
#22784 = CIRCLE ( 'NONE', #12431, 0.1023622047244094474 ) ;
#22785 = DIRECTION ( 'NONE',  ( 0.000000000000000000, -1.000000000000000000, 0.000000000000000000 ) ) ;
#22786 = ORIENTED_EDGE ( 'NONE', *, *, #17363, .T. ) ;
#22787 = B_SPLINE_CURVE_WITH_KNOTS ( 'NONE', 3,
 ( #3582, #20558, #24783, #20829, #7710, #1479, #7412, #12215, #10091, #18700 ),
 .UNSPECIFIED., .F., .F.,
 ( 4, 2, 2, 2, 4 ),
 ( 0.000000000000000000, 0.2500000000000000000, 0.5000000000000000000, 0.7500000000000000000, 1.000000000000000000 ),
 .UNSPECIFIED. ) ;
#22788 = DIRECTION ( 'NONE',  ( 0.000000000000000000, 0.000000000000000000, 1.000000000000000000 ) ) ;
#22789 = EDGE_LOOP ( 'NONE', ( #18824, #14368, #3310, #9642 ) ) ;
#22790 = DIRECTION ( 'NONE',  ( -0.000000000000000000, -0.000000000000000000, -1.000000000000000000 ) ) ;
#22791 = ORIENTED_EDGE ( 'NONE', *, *, #1132, .T. ) ;
#22792 = CARTESIAN_POINT ( 'NONE',  ( 0.1458850421962665789, 0.4296318976990154970, -1.934055118110236338 ) ) ;
#22793 = CARTESIAN_POINT ( 'NONE',  ( -0.4308867145620936534, -0.2480839813580091591, 0.1140743250925834867 ) ) ;
#22794 = CARTESIAN_POINT ( 'NONE',  ( 0.5579526598169843865, -0.3213561723284312777, 0.2359405056216625773 ) ) ;
#22795 = CARTESIAN_POINT ( 'NONE',  ( 0.04992990154984337792, 0.3112132001918756496, -3.186824010432603327 ) ) ;
#22796 = CARTESIAN_POINT ( 'NONE',  ( 0.000000000000000000, 0.000000000000000000, -0.1377952755696461029 ) ) ;
#22797 = CARTESIAN_POINT ( 'NONE',  ( 0.000000000000000000, 0.000000000000000000, -0.4724409448818898127 ) ) ;
#22798 = ORIENTED_EDGE ( 'NONE', *, *, #15270, .F. ) ;
#22799 = CARTESIAN_POINT ( 'NONE',  ( 0.1506723201675407575, 0.000000000000000000, 0.000000000000000000 ) ) ;
#22800 = ORIENTED_EDGE ( 'NONE', *, *, #3387, .F. ) ;
#22801 = AXIS2_PLACEMENT_3D ( 'NONE', #15799, #26807, #15538 ) ;
#22802 = CARTESIAN_POINT ( 'NONE',  ( 0.2952755905264887182, 0.000000000000000000, 2.090519358671640647E-11 ) ) ;
#22803 = CARTESIAN_POINT ( 'NONE',  ( -0.03937007874015747977, 0.000000000000000000, 0.000000000000000000 ) ) ;
#22804 = EDGE_CURVE ( 'NONE', #18356, #6451, #3167, .T. ) ;
#22805 = EDGE_CURVE ( 'NONE', #1952, #18288, #19094, .T. ) ;
#22806 = CARTESIAN_POINT ( 'NONE',  ( -0.2181459867477137382, -0.4514914377063456441, 0.1643955689534347675 ) ) ;
#22807 = VERTEX_POINT ( 'NONE', #27808 ) ;
#22808 = DIRECTION ( 'NONE',  ( -1.000000000000000000, 0.000000000000000000, 0.000000000000000000 ) ) ;
#22809 = APPLICATION_CONTEXT ( 'automotive_design' ) ;
#22810 = ADVANCED_FACE ( 'NONE', ( #20880 ), #24954, .T. ) ;
#22811 = EDGE_LOOP ( 'NONE', ( #16492, #3794 ) ) ;
#22812 = CARTESIAN_POINT ( 'NONE',  ( 0.1970259548082060608, 0.3996230174612934172, -1.934055118110236338 ) ) ;
#22813 = CIRCLE ( 'NONE', #10153, 1.092519685039370136 ) ;
#22814 = CARTESIAN_POINT ( 'NONE',  ( 0.3645739570812633890, 0.2796934465393874358, -1.928289503579156072 ) ) ;
#22815 = EDGE_CURVE ( 'NONE', #8924, #12716, #18996, .T. ) ;
#22816 = CONICAL_SURFACE ( 'NONE', #12451, 0.1106489370078740098, 0.08726646250000029414 ) ;
#22817 = AXIS2_PLACEMENT_3D ( 'NONE', #20980, #18845, #18997 ) ;
#22818 = EDGE_LOOP ( 'NONE', ( #4284, #7659 ) ) ;
#22819 = CARTESIAN_POINT ( 'NONE',  ( -0.3376790527244098450, -0.9256661064038090858, -0.7381404050695216101 ) ) ;
#22820 = CARTESIAN_POINT ( 'NONE',  ( -0.4986013261500205074, 0.000000000000000000, -0.05511811023622047168 ) ) ;
#22821 = DIRECTION ( 'NONE',  ( -0.9930684569432060016, -0.05876869877843096668, -0.1017903721789526900 ) ) ;
#22822 = CARTESIAN_POINT ( 'NONE',  ( 0.4600326175560532915, -0.2268096725222599475, 1.747047244094488194 ) ) ;
#22823 = AXIS2_PLACEMENT_3D ( 'NONE', #4575, #2453, #13058 ) ;
#22824 = VERTEX_POINT ( 'NONE', #6062 ) ;
#22825 = CARTESIAN_POINT ( 'NONE',  ( 0.000000000000000000, 0.000000000000000000, 0.09685039370078740717 ) ) ;
#22826 = ADVANCED_FACE ( 'NONE', ( #281 ), #652, .T. ) ;
#22827 = ORIENTED_EDGE ( 'NONE', *, *, #27018, .F. ) ;
#22828 = CARTESIAN_POINT ( 'NONE',  ( 0.1213180142433833847, 0.3572819248074460829, -3.100567304031761395 ) ) ;
#22829 = CARTESIAN_POINT ( 'NONE',  ( 0.7874015748031151229, 0.2490421840548274757, -0.2751330019808225780 ) ) ;
#22830 = FACE_OUTER_BOUND ( 'NONE', #13793, .T. ) ;
#22831 = ORIENTED_EDGE ( 'NONE', *, *, #14612, .F. ) ;
#22832 = DIRECTION ( 'NONE',  ( -0.000000000000000000, 1.000000000000000000, -0.000000000000000000 ) ) ;
#22833 = DIRECTION ( 'NONE',  ( 0.000000000000000000, -1.000000000000000000, 0.000000000000000000 ) ) ;
#22834 = CARTESIAN_POINT ( 'NONE',  ( -0.4225434286521154159, 0.3242892624566993121, 1.747047244094488194 ) ) ;
#22835 = CARTESIAN_POINT ( 'NONE',  ( 0.3858397471888846408, -0.2228126397719881469, -1.934055118110236338 ) ) ;
#22836 = ORIENTED_EDGE ( 'NONE', *, *, #15579, .T. ) ;
#22837 = VERTEX_POINT ( 'NONE', #10978 ) ;
#22838 = CARTESIAN_POINT ( 'NONE',  ( -0.2982299571017541506, 0.3545282230882351171, 0.1494804572094046713 ) ) ;
#22839 = CARTESIAN_POINT ( 'NONE',  ( -0.2165354330708661457, 0.000000000000000000, 0.000000000000000000 ) ) ;
#22840 = EDGE_CURVE ( 'NONE', #3499, #17056, #23637, .T. ) ;
#22841 = AXIS2_PLACEMENT_3D ( 'NONE', #9636, #16158, #18088 ) ;
#22842 = CARTESIAN_POINT ( 'NONE',  ( -0.02339816079119156136, -0.3574975638436101444, -3.115157480314960647 ) ) ;
#22843 = DIRECTION ( 'NONE',  ( -0.000000000000000000, -0.000000000000000000, -1.000000000000000000 ) ) ;
#22844 = CARTESIAN_POINT ( 'NONE',  ( -0.09842519685039370636, -1.570035826771653483E-17, -0.09092130223458683158 ) ) ;
#22845 = DIRECTION ( 'NONE',  ( -1.000000000000000000, 0.000000000000000000, 0.000000000000000000 ) ) ;
#22846 = EDGE_CURVE ( 'NONE', #8913, #14162, #4742, .T. ) ;
#22847 = DIRECTION ( 'NONE',  ( 0.000000000000000000, -1.000000000000000000, 0.000000000000000000 ) ) ;
#22848 = CARTESIAN_POINT ( 'NONE',  ( 0.1685339107540412551, -0.2924088307484720706, 1.973425196850393970 ) ) ;
#22849 = CARTESIAN_POINT ( 'NONE',  ( 0.3543307086614173596, -0.02319089060379044345, 1.953740157480315043 ) ) ;
#22850 = EDGE_CURVE ( 'NONE', #10277, #12575, #24930, .T. ) ;
#22851 = ORIENTED_EDGE ( 'NONE', *, *, #26400, .F. ) ;
#22852 = CARTESIAN_POINT ( 'NONE',  ( 0.03746919241557470498, 0.5708647227724243933, 0.9399606299212600602 ) ) ;
#22853 = AXIS2_PLACEMENT_3D ( 'NONE', #22600, #22740, #12008 ) ;
#22854 = DIRECTION ( 'NONE',  ( 0.000000000000000000, 0.000000000000000000, 1.000000000000000000 ) ) ;
#22855 = LINE ( 'NONE', #1514, #13960 ) ;
#22856 = EDGE_CURVE ( 'NONE', #13737, #14598, #524, .T. ) ;
#22858 = ADVANCED_FACE ( 'NONE', ( #4884 ), #8719, .T. ) ;
#22857 = DIRECTION ( 'NONE',  ( -1.224646799147353207E-16, 1.000000000000000000, 0.000000000000000000 ) ) ;
#22859 = CONICAL_SURFACE ( 'NONE', #22400, 0.4537419570391968415, 1.365720138124999927 ) ;
#22860 = CARTESIAN_POINT ( 'NONE',  ( 0.5393700787401575214, 0.000000000000000000, 0.01181102362204724393 ) ) ;
#22861 = CARTESIAN_POINT ( 'NONE',  ( -0.4777261797697566759, 0.2355331214654138305, 1.747047244094488194 ) ) ;
#22862 = CARTESIAN_POINT ( 'NONE',  ( 0.03349795313264332386, 0.5118110236220472231, 1.747047244094488194 ) ) ;
#22863 = ADVANCED_FACE ( 'NONE', ( #10841 ), #402, .T. ) ;
#22864 = AXIS2_PLACEMENT_3D ( 'NONE', #18389, #13747, #22370 ) ;
#22865 = VERTEX_POINT ( 'NONE', #24108 ) ;
#22866 = CARTESIAN_POINT ( 'NONE',  ( -0.3213305936751693626, 0.1584254766472210918, -3.115157480314960647 ) ) ;
#22867 = ORIENTED_EDGE ( 'NONE', *, *, #6112, .T. ) ;
#22868 = CARTESIAN_POINT ( 'NONE',  ( 0.3759206409296169116, 0.2989751379763687655, 0.2362204724409450174 ) ) ;
#22869 = DIRECTION ( 'NONE',  ( 0.000000000000000000, 0.000000000000000000, 1.000000000000000000 ) ) ;
#22870 = ( NAMED_UNIT ( * ) SI_UNIT ( $, .STERADIAN. ) SOLID_ANGLE_UNIT ( ) ) ;
#22871 = CARTESIAN_POINT ( 'NONE',  ( -0.5511811023622047445, 3.375010863791918375E-17, 0.9202755905511811330 ) ) ;
#22872 = FACE_BOUND ( 'NONE', #8357, .T. ) ;
#22873 = ORIENTED_EDGE ( 'NONE', *, *, #9947, .F. ) ;
#22874 = ORIENTED_EDGE ( 'NONE', *, *, #16272, .F. ) ;
#22875 = CARTESIAN_POINT ( 'NONE',  ( 0.3912931228432222075, -0.3001918266902142696, -1.569881889763779625 ) ) ;
#22876 = CARTESIAN_POINT ( 'NONE',  ( 2.664928230027803213, -0.4724409448818898127, 0.7100240035758484947 ) ) ;
#22877 = ORIENTED_EDGE ( 'NONE', *, *, #2720, .F. ) ;
#22878 = VERTEX_POINT ( 'NONE', #22121 ) ;
#22879 = DIRECTION ( 'NONE',  ( 0.2036417511401769631, -0.9790454724845838452, 1.198984999999999849E-16 ) ) ;
#22880 = CONTEXT_DEPENDENT_SHAPE_REPRESENTATION ( #26222, #1278 ) ;
#22881 = DIRECTION ( 'NONE',  ( -0.7071067818211409506, -0.7071067805519539728, 0.000000000000000000 ) ) ;
#22882 = DIRECTION ( 'NONE',  ( -1.000000000000000000, 0.000000000000000000, 0.000000000000000000 ) ) ;
#22883 = DIRECTION ( 'NONE',  ( 1.000000000000000000, 0.000000000000000000, 0.000000000000000000 ) ) ;
#22884 = PRODUCT ( 'O-Ring 36.5x2.65', 'O-Ring 36.5x2.65', '', ( #15932 ) ) ;
#22885 = EDGE_CURVE ( 'NONE', #20567, #2567, #2750, .T. ) ;
#22886 = VECTOR ( 'NONE', #10450, 39.37007874015748854 ) ;
#22887 = CARTESIAN_POINT ( 'NONE',  ( 0.000000000000000000, 0.000000000000000000, -0.1033464566929133965 ) ) ;
#22888 = UNCERTAINTY_MEASURE_WITH_UNIT (LENGTH_MEASURE( 1.000000000000000082E-05 ), #17428, 'distance_accuracy_value', 'NONE') ;
#22889 = CARTESIAN_POINT ( 'NONE',  ( -0.5241918773311228241, 0.000000000000000000, -0.2342519685039370358 ) ) ;
#22890 = PLANE ( 'NONE',  #633 ) ;
#22891 = CARTESIAN_POINT ( 'NONE',  ( 0.8549722296228741136, -0.6488494047548032384, 2.145669291338582862 ) ) ;
#22892 = CARTESIAN_POINT ( 'NONE',  ( -0.5463405388150394115, -0.3905529370662977340, 0.1756562191754173219 ) ) ;
#22893 = CARTESIAN_POINT ( 'NONE',  ( 0.1603262695921761627, -0.4410554214326614098, 0.1992150590373740204 ) ) ;
#22894 = DIRECTION ( 'NONE',  ( 1.000000000000000000, 0.000000000000000000, 0.000000000000000000 ) ) ;
#22895 = DIRECTION ( 'NONE',  ( -0.000000000000000000, -1.000000000000000000, -0.000000000000000000 ) ) ;
#22896 = ORIENTED_EDGE ( 'NONE', *, *, #11086, .T. ) ;
#22897 = AXIS2_PLACEMENT_3D ( 'NONE', #18959, #27175, #12181 ) ;
#22898 = ORIENTED_EDGE ( 'NONE', *, *, #617, .F. ) ;
#22899 = AXIS2_PLACEMENT_3D ( 'NONE', #4723, #3155, #13347 ) ;
#22900 = DIRECTION ( 'NONE',  ( 0.000000000000000000, 0.000000000000000000, 1.000000000000000000 ) ) ;
#22901 = VERTEX_POINT ( 'NONE', #15234 ) ;
#22902 = STYLED_ITEM ( 'NONE', ( #487 ), #22141 ) ;
#22903 = CARTESIAN_POINT ( 'NONE',  ( -0.2268096725200377806, -0.4600326175569655618, -1.550196850393700920 ) ) ;
#22904 = CARTESIAN_POINT ( 'NONE',  ( 0.000000000000000000, 0.000000000000000000, 0.9399606299212598381 ) ) ;
#22905 = DIRECTION ( 'NONE',  ( 0.2588190448135617161, 0.000000000000000000, 0.9659258263664945998 ) ) ;
#22906 = CARTESIAN_POINT ( 'NONE',  ( 0.06296589279854435117, 0.1968503937007873850, -3.596617852270155513 ) ) ;
#22907 = ORIENTED_EDGE ( 'NONE', *, *, #16318, .T. ) ;
#22908 = CARTESIAN_POINT ( 'NONE',  ( -0.2992781133269515892, -0.6197069291944330427, 0.3401574803149606252 ) ) ;
#22909 = ORIENTED_EDGE ( 'NONE', *, *, #18802, .T. ) ;
#22910 = CARTESIAN_POINT ( 'NONE',  ( 0.07874015748031489015, 0.000000000000000000, -0.3779527559055118058 ) ) ;
#22911 = CARTESIAN_POINT ( 'NONE',  ( 0.1247869790659374006, -0.3443449117970123208, 0.1910323753032946992 ) ) ;
#22912 = ADVANCED_FACE ( 'NONE', ( #17609, #13095 ), #13229, .T. ) ;
#22913 = CARTESIAN_POINT ( 'NONE',  ( 0.3339160553493877859, 9.254566434370079157E-06, -2.341456692880161228 ) ) ;
#22914 = DIRECTION ( 'NONE',  ( 0.000000000000000000, -1.000000000000000000, 0.000000000000000000 ) ) ;
#22915 = CARTESIAN_POINT ( 'NONE',  ( 0.3856588814717663571, -0.3381532161291455618, -1.550196850393700476 ) ) ;
#22916 = PRODUCT_DEFINITION_FORMATION_WITH_SPECIFIED_SOURCE ( 'ANY', '', #5510, .NOT_KNOWN. ) ;
#22917 = VERTEX_POINT ( 'NONE', #17474 ) ;
#22918 = CIRCLE ( 'NONE', #18837, 0.7874015748031496509 ) ;
#22919 = CARTESIAN_POINT ( 'NONE',  ( 0.4954415918535723939, -0.1327036767636087800, -1.550196850393700920 ) ) ;
#22920 = DIRECTION ( 'NONE',  ( -0.000000000000000000, -1.000000000000000000, -0.000000000000000000 ) ) ;
#22921 = CARTESIAN_POINT ( 'NONE',  ( 0.4954197419817656933, 0.2442565704126251624, 0.9202755905511811330 ) ) ;
#22922 = CARTESIAN_POINT ( 'NONE',  ( -0.3002886982018051487, -0.1727973894384558229, 0.1377952755905512416 ) ) ;
#22923 = CARTESIAN_POINT ( 'NONE',  ( -0.0006615832606325197825, 0.6212594902576319411, 0.09685039370078740717 ) ) ;
#22924 = ORIENTED_EDGE ( 'NONE', *, *, #9315, .T. ) ;
#22925 = LINE ( 'NONE', #20376, #18655 ) ;
#22926 = CARTESIAN_POINT ( 'NONE',  ( -0.1874921196022230063, 1.163150411085155822, -0.4823193919119450057 ) ) ;
#22927 = CARTESIAN_POINT ( 'NONE',  ( -0.6119360453657027854, 0.1072290460172413279, 0.2574803149606298969 ) ) ;
#22929 = ORIENTED_EDGE ( 'NONE', *, *, #13607, .F. ) ;
#22928 = AXIS2_PLACEMENT_3D ( 'NONE', #24846, #24421, #5066 ) ;
#22930 = ORIENTED_EDGE ( 'NONE', *, *, #19683, .F. ) ;
#22931 = EDGE_CURVE ( 'NONE', #20633, #26345, #17013, .T. ) ;
#22932 = CIRCLE ( 'NONE', #14375, 0.4267795243146149664 ) ;
#22933 = ORIENTED_EDGE ( 'NONE', *, *, #23684, .T. ) ;
#22934 = DIRECTION ( 'NONE',  ( -0.8660254037844383745, -0.5000000000000003331, 0.000000000000000000 ) ) ;
#22935 = VECTOR ( 'NONE', #8663, 39.37007874015748143 ) ;
#22936 = CARTESIAN_POINT ( 'NONE',  ( 0.000000000000000000, 0.000000000000000000, 0.000000000000000000 ) ) ;
#22937 = DIRECTION ( 'NONE',  ( 1.000000000000000000, 0.000000000000000000, 0.000000000000000000 ) ) ;
#22938 = ORIENTED_EDGE ( 'NONE', *, *, #5142, .F. ) ;
#22939 = CARTESIAN_POINT ( 'NONE',  ( 0.1522836969735573143, 0.000000000000000000, 0.000000000000000000 ) ) ;
#22940 = ORIENTED_EDGE ( 'NONE', *, *, #27121, .T. ) ;
#22941 = CARTESIAN_POINT ( 'NONE',  ( -0.6028220648874946797, -0.5309697779843188803, -0.9857434533500031293 ) ) ;
#22942 = CARTESIAN_POINT ( 'NONE',  ( -0.3665264996331779601, -0.2116141732283464416, 0.1377952755905511861 ) ) ;
#22943 = EDGE_CURVE ( 'NONE', #23305, #16322, #2815, .T. ) ;
#22944 = CIRCLE ( 'NONE', #25187, 0.8163976377952757435 ) ;
#22945 = FACE_OUTER_BOUND ( 'NONE', #3690, .T. ) ;
#22946 = CARTESIAN_POINT ( 'NONE',  ( 0.1522836969815822838, 0.1970374587168192970, 0.4531137400420984229 ) ) ;
#22947 = CARTESIAN_POINT ( 'NONE',  ( 0.000000000000000000, 0.5610236220472440971, 0.1771653543307086520 ) ) ;
#22948 = EDGE_LOOP ( 'NONE', ( #6199, #5195, #5631, #1449 ) ) ;
#22949 = FACE_BOUND ( 'NONE', #26387, .T. ) ;
#22950 = CYLINDRICAL_SURFACE ( 'NONE', #24140, 0.5379714048901780288 ) ;
#22951 = DIRECTION ( 'NONE',  ( 1.000000000000000000, 0.000000000000000000, 0.000000000000000000 ) ) ;
#22952 = DIRECTION ( 'NONE',  ( -1.224646799147353207E-16, 1.000000000000000000, 0.000000000000000000 ) ) ;
#22953 = DIMENSIONAL_EXPONENTS ( 1.000000000000000000, 0.000000000000000000, 0.000000000000000000, 0.000000000000000000, 0.000000000000000000, 0.000000000000000000, 0.000000000000000000 ) ;
#22954 = CIRCLE ( 'NONE', #25199, 0.1082677165354330312 ) ;
#22955 = ORIENTED_EDGE ( 'NONE', *, *, #5693, .F. ) ;
#22956 = CARTESIAN_POINT ( 'NONE',  ( 0.4446020952038907681, -0.02909913904662010317, -1.934055118110236338 ) ) ;
#22957 = VECTOR ( 'NONE', #26248, 39.37007874015748143 ) ;
#22958 = AXIS2_PLACEMENT_3D ( 'NONE', #21806, #19819, #19693 ) ;
#22959 = EDGE_CURVE ( 'NONE', #1564, #1942, #19356, .T. ) ;
#22960 = ORIENTED_EDGE ( 'NONE', *, *, #18122, .F. ) ;
#22961 = ORIENTED_EDGE ( 'NONE', *, *, #284, .T. ) ;
#22962 = ORIENTED_EDGE ( 'NONE', *, *, #15727, .T. ) ;
#22963 = CARTESIAN_POINT ( 'NONE',  ( 0.07874015748031495954, 0.1968503937007873850, -3.456364829396327387 ) ) ;
#22964 = FACE_OUTER_BOUND ( 'NONE', #4476, .T. ) ;
#22965 = CARTESIAN_POINT ( 'NONE',  ( 0.03478633594543729946, 0.5314960629921260393, 1.747047244094488194 ) ) ;
#22966 = EDGE_CURVE ( 'NONE', #17531, #10626, #8275, .T. ) ;
#22967 = ORIENTED_EDGE ( 'NONE', *, *, #26389, .F. ) ;
#22968 = ADVANCED_FACE ( 'NONE', ( #15510 ), #5109, .T. ) ;
#22969 = CARTESIAN_POINT ( 'NONE',  ( 0.2993674444872233553, -0.2296683860596848981, -3.100567304031763172 ) ) ;
#22970 = EDGE_CURVE ( 'NONE', #401, #1755, #16648, .T. ) ;
#22971 = CARTESIAN_POINT ( 'NONE',  ( 0.2078289949484098120, -0.4330237525398076270, 0.2194422276737609812 ) ) ;
#22972 = CARTESIAN_POINT ( 'NONE',  ( 0.1120675189988346587, -0.4694218845611126678, -0.3846748511993476338 ) ) ;
#22973 = ADVANCED_FACE ( 'NONE', ( #13794 ), #22692, .T. ) ;
#22974 = CARTESIAN_POINT ( 'NONE',  ( -0.3543307086614173596, 0.02319089060378165187, 1.953740157480315043 ) ) ;
#22975 = ORIENTED_EDGE ( 'NONE', *, *, #20606, .T. ) ;
#22976 = DIRECTION ( 'NONE',  ( 1.224646799147353207E-16, 1.000000000000000000, -0.000000000000000000 ) ) ;
#22977 = CIRCLE ( 'NONE', #6302, 0.08582677165167480748 ) ;
#22978 = CARTESIAN_POINT ( 'NONE',  ( 0.03532354024591712049, 0.000000000000000000, 0.000000000000000000 ) ) ;
#22980 = CARTESIAN_POINT ( 'NONE',  ( 0.03736310157557554135, 0.5708661417322835607, 0.9399606299212598381 ) ) ;
#22979 = CARTESIAN_POINT ( 'NONE',  ( 8.741913385826771462E-17, -0.1673228346456692994, 2.049113738730807629E-17 ) ) ;
#22982 = EDGE_CURVE ( 'NONE', #13505, #18491, #20340, .T. ) ;
#22981 = ( REPRESENTATION_RELATIONSHIP ('NONE','NONE', #12434, #16232 ) REPRESENTATION_RELATIONSHIP_WITH_TRANSFORMATION ( #16943 )SHAPE_REPRESENTATION_RELATIONSHIP( ) ) ;
#22983 = TOROIDAL_SURFACE ( 'NONE', #25700, 0.5393700787401575214, 0.01181102362204724393 ) ;
#22984 = PLANE ( 'NONE',  #26153 ) ;
#22985 = VERTEX_POINT ( 'NONE', #9970 ) ;
#22986 = CARTESIAN_POINT ( 'NONE',  ( -0.5511811023622047445, 0.000000000000000000, 0.000000000000000000 ) ) ;
#22987 = CARTESIAN_POINT ( 'NONE',  ( -0.7874015748031496509, 0.000000000000000000, -1.052618110236220428 ) ) ;
#22988 = CARTESIAN_POINT ( 'NONE',  ( -0.3392387706403586223, -0.1151913129404420061, -3.115157480314960647 ) ) ;
#22989 = CARTESIAN_POINT ( 'NONE',  ( -0.4330708661417322913, 0.000000000000000000, 0.000000000000000000 ) ) ;
#22990 = CIRCLE ( 'NONE', #5374, 0.3149606299212598381 ) ;
#22991 = DIRECTION ( 'NONE',  ( 0.000000000000000000, 0.000000000000000000, -1.000000000000000000 ) ) ;
#22992 = DIRECTION ( 'NONE',  ( 1.000000000000000000, 0.000000000000000000, 0.000000000000000000 ) ) ;
#22993 = PLANE ( 'NONE',  #15465 ) ;
#22994 = FACE_OUTER_BOUND ( 'NONE', #26734, .T. ) ;
#22995 = AXIS2_PLACEMENT_3D ( 'NONE', #16498, #1386, #14406 ) ;
#22996 = VERTEX_POINT ( 'NONE', #22414 ) ;
#22997 = CARTESIAN_POINT ( 'NONE',  ( -0.5525844203311578440, 0.1481265526513353969, 0.9399606299212601712 ) ) ;
#22998 = CARTESIAN_POINT ( 'NONE',  ( -0.5383572925355968319, -0.3100567972183898013, 0.09685039370078740717 ) ) ;
#22999 = DIRECTION ( 'NONE',  ( 0.000000000000000000, 0.000000000000000000, -1.000000000000000000 ) ) ;
#23000 = AXIS2_PLACEMENT_3D ( 'NONE', #19411, #13175, #13051 ) ;
#23001 = SPHERICAL_SURFACE ( 'NONE', #4719, 0.1299232283464566984 ) ;
#23002 = CARTESIAN_POINT ( 'NONE',  ( 0.5314960629921260393, 0.000000000000000000, 1.747047244094488194 ) ) ;
#23003 = CIRCLE ( 'NONE', #10814, 0.07677165354330708902 ) ;
#23004 = SHAPE_DEFINITION_REPRESENTATION ( #20617, #20013 ) ;
#23005 = DIRECTION ( 'NONE',  ( -0.000000000000000000, -1.000000000000000000, -0.000000000000000000 ) ) ;
#23006 = CARTESIAN_POINT ( 'NONE',  ( -0.4441657790107744752, -0.2564944395515745823, 1.766732283464566899 ) ) ;
#23007 = VERTEX_POINT ( 'NONE', #14232 ) ;
#23008 = ADVANCED_FACE ( 'NONE', ( #20714 ), #1093, .T. ) ;
#23009 = ORIENTED_EDGE ( 'NONE', *, *, #585, .F. ) ;
#23010 = CARTESIAN_POINT ( 'NONE',  ( 0.1580799066051618851, -0.4326553680327471785, 0.1771653543307085410 ) ) ;
#23011 = ORIENTED_EDGE ( 'NONE', *, *, #8672, .T. ) ;
#23012 = CARTESIAN_POINT ( 'NONE',  ( 0.3882259019049796867, 0.3087756353516248331, 0.1734435147392032195 ) ) ;
#23013 = CARTESIAN_POINT ( 'NONE',  ( 0.4535326485287340947, 0.08054850140356764610, 0.1903859678014195589 ) ) ;
#23014 = ADVANCED_FACE ( 'NONE', ( #9396 ), #11530, .T. ) ;
#23015 = DIRECTION ( 'NONE',  ( 0.000000000000000000, 0.000000000000000000, -1.000000000000000000 ) ) ;
#23016 = ORIENTED_EDGE ( 'NONE', *, *, #22931, .F. ) ;
#23017 = CARTESIAN_POINT ( 'NONE',  ( -0.3912931228432124930, 0.3001918266902225407, -1.550196850393700920 ) ) ;
#23018 = FACE_BOUND ( 'NONE', #22811, .T. ) ;
#23019 = EDGE_LOOP ( 'NONE', ( #7086, #8778, #9674, #11666, #13065 ) ) ;
#23020 = ORIENTED_EDGE ( 'NONE', *, *, #26703, .T. ) ;
#23021 = VECTOR ( 'NONE', #27641, 39.37007874015748143 ) ;
#23022 = CARTESIAN_POINT ( 'NONE',  ( 0.3334645669291338987, -1.091522395027023640, -0.7267332332655965788 ) ) ;
#23023 = CIRCLE ( 'NONE', #472, 0.1673228346456692994 ) ;
#23024 = CARTESIAN_POINT ( 'NONE',  ( -0.06889763779527552368, 0.000000000000000000, -0.02362204724409468909 ) ) ;
#23025 = FACE_OUTER_BOUND ( 'NONE', #20276, .T. ) ;
#23026 = DIRECTION ( 'NONE',  ( 0.000000000000000000, 1.000000000000000000, 0.000000000000000000 ) ) ;
#23027 = EDGE_CURVE ( 'NONE', #5267, #10260, #7845, .T. ) ;
#23028 = B_SPLINE_CURVE_WITH_KNOTS ( 'NONE', 3,
 ( #1963, #25699, #14982, #2105, #297, #10572 ),
 .UNSPECIFIED., .F., .F.,
 ( 4, 2, 4 ),
 ( 0.4045103800603460087, 0.4064350009536160102, 0.4083596218468860117 ),
 .UNSPECIFIED. ) ;
#23029 = VERTEX_POINT ( 'NONE', #18139 ) ;
#23030 = CARTESIAN_POINT ( 'NONE',  ( -0.3334645669291338987, 0.000000000000000000, -1.052618110236220428 ) ) ;
#23031 = DIRECTION ( 'NONE',  ( 0.000000000000000000, 0.000000000000000000, 1.000000000000000000 ) ) ;
#23032 = CARTESIAN_POINT ( 'NONE',  ( -0.4468450976383792628, -0.7637389252159438868, -0.01428724896956997704 ) ) ;
#23033 = ( BOUNDED_CURVE ( )  B_SPLINE_CURVE ( 2, ( #17623, #17355, #26239 ),
 .UNSPECIFIED., .F., .T. ) 
 B_SPLINE_CURVE_WITH_KNOTS ( ( 3, 3 ),
 ( 0.000000000000000000, 0.5842180690389598974 ),
 .UNSPECIFIED. ) 
 CURVE ( )  GEOMETRIC_REPRESENTATION_ITEM ( )  RATIONAL_B_SPLINE_CURVE ( ( 1.000000000000000000, 1.154700538379249908, 1.000000000000000000 ) ) 
 REPRESENTATION_ITEM ( '' )  ) ;
#23034 = DIRECTION ( 'NONE',  ( 0.000000000000000000, -0.8660254037844384856, -0.5000000000000003331 ) ) ;
#23035 = CARTESIAN_POINT ( 'NONE',  ( -0.5905511811023621549, 7.232166136696967594E-17, 1.707677165389662743 ) ) ;
#23036 = CARTESIAN_POINT ( 'NONE',  ( -0.09842519685039370636, -1.570035826771653483E-17, -0.09092130223458683158 ) ) ;
#23037 = EDGE_CURVE ( 'NONE', #8378, #26227, #13940, .T. ) ;
#23038 = TOROIDAL_SURFACE ( 'NONE', #14477, 0.5610236220472440971, 0.1003937007874015908 ) ;
#23040 = ADVANCED_FACE ( 'NONE', ( #15912, #9690 ), #18430, .T. ) ;
#23039 = VERTEX_POINT ( 'NONE', #20431 ) ;
#23041 = VERTEX_POINT ( 'NONE', #5603 ) ;
#23042 = EDGE_CURVE ( 'NONE', #3818, #2008, #2472, .T. ) ;
#23043 = ORIENTED_EDGE ( 'NONE', *, *, #416, .T. ) ;
#23044 = CIRCLE ( 'NONE', #480, 0.6299212598425196763 ) ;
#23045 = CARTESIAN_POINT ( 'NONE',  ( -0.4069448477569433953, -0.3121994997578269593, -1.550196850393700920 ) ) ;
#23046 = CARTESIAN_POINT ( 'NONE',  ( 0.000000000000000000, 0.000000000000000000, 0.1771653543307086520 ) ) ;
#23047 = DIRECTION ( 'NONE',  ( 0.000000000000000000, 0.000000000000000000, 1.000000000000000000 ) ) ;
#23048 = CARTESIAN_POINT ( 'NONE',  ( 0.000000000000000000, 0.5511811023622047445, 0.2637795275590551491 ) ) ;
#23049 = VERTEX_POINT ( 'NONE', #24654 ) ;
#23050 = CARTESIAN_POINT ( 'NONE',  ( 0.000000000000000000, 0.1968503937007874127, 0.000000000000000000 ) ) ;
#23051 = DIRECTION ( 'NONE',  ( -1.000000000000000000, 0.000000000000000000, 0.000000000000000000 ) ) ;
#23052 = VERTEX_POINT ( 'NONE', #11669 ) ;
#23053 = FILL_AREA_STYLE_COLOUR ( '', #12141 ) ;
#23054 = CARTESIAN_POINT ( 'NONE',  ( -0.0005789221761808661720, 0.4692909815006409691, 0.1992125984251968684 ) ) ;
#23055 = PLANE ( 'NONE',  #23995 ) ;
#23056 = CARTESIAN_POINT ( 'NONE',  ( -0.4442166144910411063, -0.2564158049327064925, -1.550196850393700920 ) ) ;
#23057 = B_SPLINE_CURVE_WITH_KNOTS ( 'NONE', 3,
 ( #18479, #12002, #14572, #10434, #5650, #21035, #20621, #18906 ),
 .UNSPECIFIED., .F., .F.,
 ( 4, 2, 2, 4 ),
 ( 0.000000000000000000, 0.1250000000000000555, 0.2500000000000001110, 0.5000000000000000000 ),
 .UNSPECIFIED. ) ;
#23058 = EDGE_CURVE ( 'NONE', #3542, #12477, #5315, .T. ) ;
#23059 = AXIS2_PLACEMENT_3D ( 'NONE', #11500, #13757, #22377 ) ;
#23060 = CARTESIAN_POINT ( 'NONE',  ( -0.3149606299212598381, 0.5905511811023621549, 0.000000000000000000 ) ) ;
#23061 = ORIENTED_EDGE ( 'NONE', *, *, #23097, .T. ) ;
#23062 = CARTESIAN_POINT ( 'NONE',  ( -0.6478824768862475603, 0.1135474080046062623, 0.1461456498260605696 ) ) ;
#23063 = CARTESIAN_POINT ( 'NONE',  ( 0.4068916527365293856, -0.3122765577857888331, -1.550196850393700920 ) ) ;
#23064 = ORIENTED_EDGE ( 'NONE', *, *, #20692, .T. ) ;
#23065 = CARTESIAN_POINT ( 'NONE',  ( 0.3007905576423883232, 0.1482986320106616795, 1.953740157480315043 ) ) ;
#23066 = CARTESIAN_POINT ( 'NONE',  ( 0.5085118447796559416, -0.06699507805604926203, -1.550196850393700920 ) ) ;
#23067 = CARTESIAN_POINT ( 'NONE',  ( -0.4446020952038907681, 0.000000000000000000, -1.934055118110236338 ) ) ;
#23068 = CARTESIAN_POINT ( 'NONE',  ( -0.5708661417322835607, 0.000000000000000000, 0.9399606299212598381 ) ) ;
#23069 = FACE_OUTER_BOUND ( 'NONE', #946, .T. ) ;
#23070 = DIRECTION ( 'NONE',  ( -0.7071067805519565264, 0.000000000000000000, -0.7071067818211385081 ) ) ;
#23071 = ORIENTED_EDGE ( 'NONE', *, *, #23983, .T. ) ;
#23072 = CARTESIAN_POINT ( 'NONE',  ( -0.2305483297598421022, -0.4797636960996590760, 0.3401591244667909186 ) ) ;
#23073 = EDGE_CURVE ( 'NONE', #20420, #20990, #13938, .T. ) ;
#23074 = ORIENTED_EDGE ( 'NONE', *, *, #23876, .T. ) ;
#23075 = ADVANCED_FACE ( 'NONE', ( #6192 ), #19578, .F. ) ;
#23076 = DIRECTION ( 'NONE',  ( 0.000000000000000000, 0.000000000000000000, 1.000000000000000000 ) ) ;
#23077 = DIRECTION ( 'NONE',  ( -0.9575713608335526539, -0.2881962680386024878, 2.462036256411297774E-17 ) ) ;
#23078 = DIRECTION ( 'NONE',  ( 0.000000000000000000, -1.000000000000000000, 0.000000000000000000 ) ) ;
#23079 = CARTESIAN_POINT ( 'NONE',  ( 0.3242876858384301508, -0.4225410690758546473, 1.747047244094488194 ) ) ;
#23080 = ORIENTED_EDGE ( 'NONE', *, *, #25526, .F. ) ;
#23081 = CARTESIAN_POINT ( 'NONE',  ( -0.6299212598425196763, -0.4724409448818898127, 0.8182917201112794858 ) ) ;
#23082 = VERTEX_POINT ( 'NONE', #2056 ) ;
#23083 = AXIS2_PLACEMENT_3D ( 'NONE', #20562, #26766, #22396 ) ;
#23084 = DIRECTION ( 'NONE',  ( 0.000000000000000000, 0.000000000000000000, 1.000000000000000000 ) ) ;
#23085 = DIRECTION ( 'NONE',  ( 0.000000000000000000, 1.000000000000000000, 0.000000000000000000 ) ) ;
#23086 = CARTESIAN_POINT ( 'NONE',  ( -0.5656588455786464298, -0.5969388012308868285, -0.9446411342982088399 ) ) ;
#23087 = LINE ( 'NONE', #25333, #9927 ) ;
#23088 = DIRECTION ( 'NONE',  ( 0.000000000000000000, 0.000000000000000000, -1.000000000000000000 ) ) ;
#23089 = CARTESIAN_POINT ( 'NONE',  ( -0.4895985792973480133, 1.185352029804633059E-17, 0.09679133858267717494 ) ) ;
#23090 = ORIENTED_EDGE ( 'NONE', *, *, #3378, .F. ) ;
#23091 = ( NAMED_UNIT ( * ) SI_UNIT ( $, .STERADIAN. ) SOLID_ANGLE_UNIT ( ) ) ;
#23092 = DIRECTION ( 'NONE',  ( -0.000000000000000000, -1.000000000000000000, -0.000000000000000000 ) ) ;
#23093 = DIRECTION ( 'NONE',  ( 0.000000000000000000, 1.000000000000000000, 0.000000000000000000 ) ) ;
#23094 = PRESENTATION_STYLE_ASSIGNMENT (( #14053 ) ) ;
#23095 = CARTESIAN_POINT ( 'NONE',  ( 0.1585706980422492418, -0.4669911931914798586, -1.569881889763779625 ) ) ;
#23096 = VERTEX_POINT ( 'NONE', #5753 ) ;
#23097 = EDGE_CURVE ( 'NONE', #15651, #25542, #12374, .T. ) ;
#23098 = CARTESIAN_POINT ( 'NONE',  ( 0.4303822302054278182, -0.1152775731717046309, -1.934055118110236338 ) ) ;
#23099 = CIRCLE ( 'NONE', #24892, 0.5241918773311228241 ) ;
#23100 = EDGE_LOOP ( 'NONE', ( #7762, #16769, #16827, #7249 ) ) ;
#23101 = VERTEX_POINT ( 'NONE', #21133 ) ;
#23102 = ORIENTED_EDGE ( 'NONE', *, *, #16085, .F. ) ;
#23104 = EDGE_LOOP ( 'NONE', ( #27350, #7061, #2635, #19704, #10648 ) ) ;
#23103 = EDGE_CURVE ( 'NONE', #1637, #8715, #15015, .T. ) ;
#23105 = CARTESIAN_POINT ( 'NONE',  ( -0.5833277509429386498, -0.2585366369247649732, 0.2102047045095200573 ) ) ;
#23106 = CARTESIAN_POINT ( 'NONE',  ( -0.06957181182498481387, 0.5280699926563169333, 1.747047244094488194 ) ) ;
#23107 = ORIENTED_EDGE ( 'NONE', *, *, #25911, .T. ) ;
#23108 = FACE_OUTER_BOUND ( 'NONE', #9775, .T. ) ;
#23109 = ORIENTED_EDGE ( 'NONE', *, *, #20124, .T. ) ;
#23110 = CARTESIAN_POINT ( 'NONE',  ( 0.1886891683788910479, -0.3267488823401750730, -3.100567304031762284 ) ) ;
#23111 = CARTESIAN_POINT ( 'NONE',  ( -0.09193127540133588793, -0.3429876364231727037, 1.953740157480314821 ) ) ;
#23112 = CARTESIAN_POINT ( 'NONE',  ( 0.3018020646414488750, 0.3593743330771480560, 0.1992150590373740204 ) ) ;
#23113 = PRODUCT ( 'Barrel Cam', 'Barrel Cam', '', ( #21981 ) ) ;
#23114 = CARTESIAN_POINT ( 'NONE',  ( -0.08294224740493465198, -0.3300511624395449095, 0.04829813222822094965 ) ) ;
#23115 = CARTESIAN_POINT ( 'NONE',  ( -0.3074993854542729665, -0.1775730735577446262, 1.953740157480315043 ) ) ;
#23116 = ORIENTED_EDGE ( 'NONE', *, *, #1068, .F. ) ;
#23117 = AXIS2_PLACEMENT_3D ( 'NONE', #24557, #848, #17783 ) ;
#23118 = CARTESIAN_POINT ( 'NONE',  ( -0.5336559655304955463, -0.2766137621800717206, -0.2845086883298418856 ) ) ;
#23120 = CARTESIAN_POINT ( 'NONE',  ( 0.4954197419818043846, -0.2442565704126259674, 0.9399606299212598381 ) ) ;
#23119 = DIRECTION ( 'NONE',  ( 0.000000000000000000, 0.000000000000000000, -1.000000000000000000 ) ) ;
#23121 = ORIENTED_EDGE ( 'NONE', *, *, #1320, .F. ) ;
#23122 = ORIENTED_EDGE ( 'NONE', *, *, #2323, .F. ) ;
#23123 = ORIENTED_EDGE ( 'NONE', *, *, #16043, .F. ) ;
#23124 = CARTESIAN_POINT ( 'NONE',  ( 0.000000000000000000, 0.000000000000000000, 0.1377952755905511861 ) ) ;
#23125 = DIRECTION ( 'NONE',  ( -0.9396926207859083169, -0.3420201433256692125, 0.000000000000000000 ) ) ;
#23126 = AXIS2_PLACEMENT_3D ( 'NONE', #25514, #16306, #9362 ) ;
#23127 = AXIS2_PLACEMENT_3D ( 'NONE', #19436, #1783, #131 ) ;
#23128 = CARTESIAN_POINT ( 'NONE',  ( 0.2693339498142252042, 0.2362439534887496861, -3.115157480314960647 ) ) ;
#23129 = CARTESIAN_POINT ( 'NONE',  ( -0.1442704874421230077, -0.5368353335967094297, 0.9202755905511812440 ) ) ;
#23130 = DIRECTION ( 'NONE',  ( 0.000000000000000000, 0.000000000000000000, -1.000000000000000000 ) ) ;
#23131 = EDGE_CURVE ( 'NONE', #3232, #11793, #20858, .T. ) ;
#23132 = DIRECTION ( 'NONE',  ( 0.000000000000000000, 7.180547322999998243E-06, -0.9999999999742198442 ) ) ;
#23133 = CARTESIAN_POINT ( 'NONE',  ( 0.0006681923949024700608, 0.6336721034114674023, 0.2481708550952533565 ) ) ;
#23134 = ADVANCED_FACE ( 'NONE', ( #23270 ), #17257, .F. ) ;
#23135 = ORIENTED_EDGE ( 'NONE', *, *, #16858, .T. ) ;
#23136 = CARTESIAN_POINT ( 'NONE',  ( -0.5130713940405708939, 0.2530774914993670910, 0.9399606299212600602 ) ) ;
#23137 = FACE_OUTER_BOUND ( 'NONE', #4357, .T. ) ;
#23138 = CONICAL_SURFACE ( 'NONE', #14587, 1.112204724409448842, 0.7853981625000011624 ) ;
#23139 = CARTESIAN_POINT ( 'NONE',  ( 0.000000000000000000, 0.000000000000000000, -6.010066929133858501E-17 ) ) ;
#23140 = EDGE_CURVE ( 'NONE', #11663, #20576, #1732, .T. ) ;
#23141 = CARTESIAN_POINT ( 'NONE',  ( 0.03937007874015747977, 4.339299682018180063E-17, 0.3346456692913385988 ) ) ;
#23142 = CARTESIAN_POINT ( 'NONE',  ( 0.07870736637777375755, 0.2165354330708660624, -3.608715228343986503 ) ) ;
#23143 = CARTESIAN_POINT ( 'NONE',  ( -0.3012109481301850633, 0.3598698725862389813, 0.07637795275590551769 ) ) ;
#23144 = CARTESIAN_POINT ( 'NONE',  ( -0.2268599607415002495, -0.6212949646971562823, 0.1926811207740130039 ) ) ;
#23145 = CARTESIAN_POINT ( 'NONE',  ( -0.1649135259617057203, -0.4856708409200641841, 1.766732283464566899 ) ) ;
#23146 = ORIENTED_EDGE ( 'NONE', *, *, #17288, .T. ) ;
#23147 = AXIS2_PLACEMENT_3D ( 'NONE', #13319, #2571, #17940 ) ;
#23148 = DIRECTION ( 'NONE',  ( 1.000000000000000000, 0.000000000000000000, -0.000000000000000000 ) ) ;
#23149 = ORIENTED_EDGE ( 'NONE', *, *, #15985, .F. ) ;
#23150 = CARTESIAN_POINT ( 'NONE',  ( 0.2309201403895322358, -0.4006498629591506155, -1.928289503579156960 ) ) ;
#23151 = CARTESIAN_POINT ( 'NONE',  ( -0.02559055118110236185, 0.000000000000000000, 0.000000000000000000 ) ) ;
#23152 = CARTESIAN_POINT ( 'NONE',  ( -0.0004974201395674844595, 0.3464563358313497154, 0.1276989850599299925 ) ) ;
#23153 = B_SPLINE_CURVE_WITH_KNOTS ( 'NONE', 2,
 ( #6011, #10506, #8126 ),
 .UNSPECIFIED., .F., .F.,
 ( 3, 3 ),
 ( 0.000000000000000000, 1.000000000000000000 ),
 .UNSPECIFIED. ) ;
#23154 = CARTESIAN_POINT ( 'NONE',  ( -0.3324885138898239778, 0.04380447413658877104, 1.973425196850393970 ) ) ;
#23155 = ORIENTED_EDGE ( 'NONE', *, *, #14340, .T. ) ;
#23156 = ORIENTED_EDGE ( 'NONE', *, *, #6809, .T. ) ;
#23157 = CARTESIAN_POINT ( 'NONE',  ( -0.3001918266902322552, -0.3912931228432061648, -1.550196850393700920 ) ) ;
#23158 = CARTESIAN_POINT ( 'NONE',  ( -0.09842519685039370636, -0.1673228346456692994, 2.049113738730807629E-17 ) ) ;
#23159 = ORIENTED_EDGE ( 'NONE', *, *, #10017, .T. ) ;
#23160 = AXIS2_PLACEMENT_3D ( 'NONE', #1697, #25713, #5809 ) ;
#23161 = CONICAL_SURFACE ( 'NONE', #20890, 0.4537419570391968415, 1.365720138124999927 ) ;
#23162 = EDGE_CURVE ( 'NONE', #17199, #14009, #20219, .T. ) ;
#23163 = ITEM_DEFINED_TRANSFORMATION ( 'NONE', 'NONE', #2161,  #11588 ) ;
#23164 = CARTESIAN_POINT ( 'NONE',  ( 0.000000000000000000, -4.081314960629921056E-17, -0.1692378991623492424 ) ) ;
#23165 = LINE ( 'NONE', #11998, #21583 ) ;
#23166 = CARTESIAN_POINT ( 'NONE',  ( 0.5379168165870276130, -0.3108204284649302984, 0.09684793308443542803 ) ) ;
#23167 = DIRECTION ( 'NONE',  ( 0.000000000000000000, 0.000000000000000000, -1.000000000000000000 ) ) ;
#23168 = EDGE_CURVE ( 'NONE', #18177, #27722, #17524, .T. ) ;
#23169 = AXIS2_PLACEMENT_3D ( 'NONE', #16382, #3507, #12006 ) ;
#23170 = ORIENTED_EDGE ( 'NONE', *, *, #18065, .F. ) ;
#23171 = CARTESIAN_POINT ( 'NONE',  ( -0.3222028160008074682, 0.3833711078595924970, 0.2574819596263889787 ) ) ;
#23172 = EDGE_CURVE ( 'NONE', #13858, #372, #9373, .T. ) ;
#23173 = CARTESIAN_POINT ( 'NONE',  ( 0.1518453843511950729, -0.4909359254672716610, -0.05583672882996244813 ) ) ;
#23174 = CARTESIAN_POINT ( 'NONE',  ( -0.3661417322834645272, 0.9448818897637796255, -1.639108661417322569E-17 ) ) ;
#23175 = DIRECTION ( 'NONE',  ( 0.000000000000000000, 1.000000000000000000, 0.000000000000000000 ) ) ;
#23176 = CARTESIAN_POINT ( 'NONE',  ( -0.5756876931373007267, -0.2855297575254043818, 0.2042278449590817502 ) ) ;
#23177 = CARTESIAN_POINT ( 'NONE',  ( 0.000000000000000000, 0.9055118110236217710, 0.000000000000000000 ) ) ;
#23178 = ADVANCED_FACE ( 'NONE', ( #6178 ), #10389, .T. ) ;
#23179 = CARTESIAN_POINT ( 'NONE',  ( 0.000000000000000000, 0.000000000000000000, -0.01377952755905511792 ) ) ;
#23180 = FACE_BOUND ( 'NONE', #8885, .T. ) ;
#23181 = CIRCLE ( 'NONE', #3297, 0.2952755905264887182 ) ;
#23182 = EDGE_CURVE ( 'NONE', #24915, #8070, #15292, .T. ) ;
#23183 = AXIS2_PLACEMENT_3D ( 'NONE', #11331, #27009, #13580 ) ;
#23184 = LINE ( 'NONE', #8345, #22670 ) ;
#23185 = ORIENTED_EDGE ( 'NONE', *, *, #4130, .F. ) ;
#23186 = EDGE_LOOP ( 'NONE', ( #7429, #19284, #17638, #17470 ) ) ;
#23187 = EDGE_CURVE ( 'NONE', #10834, #26561, #25228, .T. ) ;
#23188 = ORIENTED_EDGE ( 'NONE', *, *, #8343, .T. ) ;
#23189 = CARTESIAN_POINT ( 'NONE',  ( -0.3855916753034467903, -0.3382184156749090675, -1.550196850393700920 ) ) ;
#23190 = DIRECTION ( 'NONE',  ( 0.000000000000000000, 0.000000000000000000, -1.000000000000000000 ) ) ;
#23191 = DIRECTION ( 'NONE',  ( 1.000000000000000000, 0.000000000000000000, 0.000000000000000000 ) ) ;
#23192 = TOROIDAL_SURFACE ( 'NONE', #1516, 0.4173228346456693272, 0.02362204724409448786 ) ;
#23193 = CARTESIAN_POINT ( 'NONE',  ( -0.1775991818008739453, 0.5230301363771271417, 0.9202755905511811330 ) ) ;
#23194 = ORIENTED_EDGE ( 'NONE', *, *, #24462, .F. ) ;
#23195 = CARTESIAN_POINT ( 'NONE',  ( -0.09842519685039370636, -0.07874015748031495954, 0.04546065111729338803 ) ) ;
#23196 = VERTEX_POINT ( 'NONE', #1639 ) ;
#23197 = ( LENGTH_UNIT ( ) NAMED_UNIT ( * ) SI_UNIT ( $, .METRE. ) ) ;
#23198 = DIRECTION ( 'NONE',  ( -1.000000000000000000, -7.017815999999999636E-18, 0.000000000000000000 ) ) ;
#23199 = AXIS2_PLACEMENT_3D ( 'NONE', #27440, #9915, #27163 ) ;
#23200 = CARTESIAN_POINT ( 'NONE',  ( -0.4055118110236220486, -0.4724409448818898127, 0.8182917201112794858 ) ) ;
#23201 = EDGE_LOOP ( 'NONE', ( #11562, #8269, #3176, #27441, #1976, #2618, #23289, #8538 ) ) ;
#23202 = CARTESIAN_POINT ( 'NONE',  ( 0.1490609433615242285, 0.2393035190771452825, -0.4144858534716441278 ) ) ;
#23203 = ORIENTED_EDGE ( 'NONE', *, *, #13983, .F. ) ;
#23204 = CARTESIAN_POINT ( 'NONE',  ( 0.08676778863010879694, -0.3239425792934411685, 1.973425196850393970 ) ) ;
#23205 = CARTESIAN_POINT ( 'NONE',  ( -0.1649135259639108730, -0.4856708409191554665, -1.550196850393700920 ) ) ;
#23206 = ADVANCED_FACE ( 'NONE', ( #5895, #16757 ), #18858, .T. ) ;
#23207 = CARTESIAN_POINT ( 'NONE',  ( 0.0005939837304750000086, 0.5007870493127504208, 0.2574803149606298969 ) ) ;
#23208 = CIRCLE ( 'NONE', #10565, 0.06889763779527552368 ) ;
#23209 = CARTESIAN_POINT ( 'NONE',  ( 0.3362148458988353239, 0.4382482975805538361, 0.9399606299212598381 ) ) ;
#23210 = CARTESIAN_POINT ( 'NONE',  ( -0.07874015748031495954, 0.04546065111729338803, -0.3779527559055118058 ) ) ;
#23211 = CIRCLE ( 'NONE', #13252, 0.5241918773311228241 ) ;
#23212 = CARTESIAN_POINT ( 'NONE',  ( 2.531258147843938596E-16, 0.1574803148899641958, 2.066929133858267598 ) ) ;
#23213 = ORIENTED_EDGE ( 'NONE', *, *, #14207, .T. ) ;
#23214 = CARTESIAN_POINT ( 'NONE',  ( 0.09275304139143687732, 0.3460530745557324206, -3.115157480314960647 ) ) ;
#23215 = EDGE_CURVE ( 'NONE', #15651, #22705, #1917, .T. ) ;
#23216 = DIRECTION ( 'NONE',  ( 0.000000000000000000, 0.000000000000000000, 1.000000000000000000 ) ) ;
#23217 = CARTESIAN_POINT ( 'NONE',  ( 0.4776874499715109135, 0.2356229156554291715, 1.747047244094487528 ) ) ;
#23218 = AXIS2_PLACEMENT_3D ( 'NONE', #7918, #5375, #11863 ) ;
#23219 = ORIENTED_EDGE ( 'NONE', *, *, #2597, .F. ) ;
#23220 = CARTESIAN_POINT ( 'NONE',  ( -0.4600326175569863785, 0.2268096725200117181, -1.550196850393700920 ) ) ;
#23221 = CARTESIAN_POINT ( 'NONE',  ( 2.025004910739483854, 0.000000000000000000, 0.4528769840262404922 ) ) ;
#23222 = CARTESIAN_POINT ( 'NONE',  ( 2.185478346456692557E-17, -4.034314960629921845E-17, -0.1625845656552793450 ) ) ;
#23223 = DIRECTION ( 'NONE',  ( -1.000000000000000000, 0.000000000000000000, 0.000000000000000000 ) ) ;
#23224 = CARTESIAN_POINT ( 'NONE',  ( -0.1711654736996711390, -0.5043865966254131861, 1.747047244094488194 ) ) ;
#23225 = ORIENTED_EDGE ( 'NONE', *, *, #4810, .F. ) ;
#23226 = CARTESIAN_POINT ( 'NONE',  ( -0.5692984878077121946, -0.5056997808577781139, 0.9923580223634099751 ) ) ;
#23227 = ORIENTED_EDGE ( 'NONE', *, *, #3685, .T. ) ;
#23228 = AXIS2_PLACEMENT_3D ( 'NONE', #13256, #25983, #8878 ) ;
#23229 = DIRECTION ( 'NONE',  ( -0.1736481776669310251, -0.9848077530122080203, 0.000000000000000000 ) ) ;
#23230 = CONICAL_SURFACE ( 'NONE', #24095, 0.1318897637674583401, 0.5235987755982981495 ) ;
#23231 = PLANE ( 'NONE',  #13996 ) ;
#23232 = DIRECTION ( 'NONE',  ( 0.000000000000000000, -1.000000000000000000, 0.000000000000000000 ) ) ;
#23233 = ORIENTED_EDGE ( 'NONE', *, *, #3626, .T. ) ;
#23234 = CARTESIAN_POINT ( 'NONE',  ( 0.000000000000000000, 0.000000000000000000, 0.000000000000000000 ) ) ;
#23235 = DIRECTION ( 'NONE',  ( 1.000000000000000000, 0.000000000000000000, 0.000000000000000000 ) ) ;
#23236 = EDGE_CURVE ( 'NONE', #15131, #12919, #6387, .T. ) ;
#23237 = CARTESIAN_POINT ( 'NONE',  ( 0.000000000000000000, 0.4692913385826771866, -3.278217716535432842E-17 ) ) ;
#23238 = ORIENTED_EDGE ( 'NONE', *, *, #21675, .T. ) ;
#23239 = CARTESIAN_POINT ( 'NONE',  ( -0.3102827802123664935, -0.1791101711252766349, -3.115157480314960647 ) ) ;
#23240 = FACE_OUTER_BOUND ( 'NONE', #11247, .T. ) ;
#23241 = ADVANCED_FACE ( 'NONE', ( #16904 ), #3237, .T. ) ;
#23242 = CONICAL_SURFACE ( 'NONE', #11046, 0.1074461786882927178, 1.047197550000000144 ) ;
#23243 = UNCERTAINTY_MEASURE_WITH_UNIT (LENGTH_MEASURE( 1.000000000000000082E-05 ), #25683, 'distance_accuracy_value', 'NONE') ;
#23244 = CARTESIAN_POINT ( 'NONE',  ( 0.2761764805255846333, -0.3599896729929844552, -1.934055118110236338 ) ) ;
#23245 = CARTESIAN_POINT ( 'NONE',  ( 0.4121342552748372690, -0.2031943647053953139, -1.928289503579153630 ) ) ;
#23246 = EDGE_CURVE ( 'NONE', #12575, #16738, #25310, .T. ) ;
#23247 = AXIS2_PLACEMENT_3D ( 'NONE', #25919, #10376, #6170 ) ;
#23248 = ORIENTED_EDGE ( 'NONE', *, *, #3359, .F. ) ;
#23249 = AXIS2_PLACEMENT_3D ( 'NONE', #26338, #639, #23823 ) ;
#23250 = CARTESIAN_POINT ( 'NONE',  ( -0.5172021183779732523, -0.3756403699547334885, -0.1539580800082084311 ) ) ;
#23251 = CARTESIAN_POINT ( 'NONE',  ( -0.4004221243553304777, 0.3512268162760389667, 1.747047244094488194 ) ) ;
#23252 = B_SPLINE_CURVE_WITH_KNOTS ( 'NONE', 3,
 ( #17114, #21492, #17250, #25194, #7837, #10749, #27191, #1334 ),
 .UNSPECIFIED., .F., .F.,
 ( 4, 2, 2, 4 ),
 ( 0.000000000000000000, 0.1250000000000000833, 0.2500000000000001665, 0.5000000000000000000 ),
 .UNSPECIFIED. ) ;
#23253 = ORIENTED_EDGE ( 'NONE', *, *, #22280, .T. ) ;
#23254 = VERTEX_POINT ( 'NONE', #1575 ) ;
#23255 = ( BOUNDED_CURVE ( )  B_SPLINE_CURVE ( 2, ( #7262, #7000, #22383 ),
 .UNSPECIFIED., .F., .F. ) 
 B_SPLINE_CURVE_WITH_KNOTS ( ( 3, 3 ),
 ( 0.1168436138077914160, 0.2336872276155829709 ),
 .UNSPECIFIED. ) 
 CURVE ( )  GEOMETRIC_REPRESENTATION_ITEM ( )  RATIONAL_B_SPLINE_CURVE ( ( 1.077350269189623067, 1.077350269189623067, 1.000000000000000000 ) ) 
 REPRESENTATION_ITEM ( '' )  ) ;
#23256 = DIRECTION ( 'NONE',  ( 0.000000000000000000, 1.000000000000000000, 0.000000000000000000 ) ) ;
#23257 = CARTESIAN_POINT ( 'NONE',  ( -0.2161891097064467526, -0.2816986811833155913, 1.953740157480314821 ) ) ;
#23258 = CARTESIAN_POINT ( 'NONE',  ( 0.000000000000000000, 0.1136516277932338587, -0.1968503937007874127 ) ) ;
#23259 = CARTESIAN_POINT ( 'NONE',  ( 0.4417530401346461688, 0.05811992390560041799, -1.934055118110236116 ) ) ;
#23260 = CIRCLE ( 'NONE', #11067, 0.03937007874015744507 ) ;
#23261 = CARTESIAN_POINT ( 'NONE',  ( -0.3362336590883616139, -0.1141709026133614219, 1.953740157480315043 ) ) ;
#23262 = ORIENTED_EDGE ( 'NONE', *, *, #17412, .T. ) ;
#23263 = EDGE_LOOP ( 'NONE', ( #8213, #18155 ) ) ;
#23264 = FACE_BOUND ( 'NONE', #23355, .T. ) ;
#23265 = VERTEX_POINT ( 'NONE', #4122 ) ;
#23267 = CARTESIAN_POINT ( 'NONE',  ( -0.5671862884095228985, -0.07472527936312044206, 0.9399606299212598381 ) ) ;
#23266 = CARTESIAN_POINT ( 'NONE',  ( -0.2303471512294322787, -0.4798602677570401598, 0.1322834645669291320 ) ) ;
#23268 = SPHERICAL_SURFACE ( 'NONE', #22559, 0.1003956692913385851 ) ;
#23269 = EDGE_LOOP ( 'NONE', ( #4610, #17340, #2215, #14699, #10174, #27172, #3533, #21565, #9322, #22851, #318, #21853, #14483, #27390 ) ) ;
#23270 = FACE_OUTER_BOUND ( 'NONE', #19609, .T. ) ;
#23271 = DIRECTION ( 'NONE',  ( 0.000000000000000000, -7.180547322999999937E-06, -0.9999999999742198442 ) ) ;
#23272 = VECTOR ( 'NONE', #17672, 39.37007874015748143 ) ;
#23273 = CARTESIAN_POINT ( 'NONE',  ( -0.1584254766472190379, -0.3213305936751582048, -3.115157480314960647 ) ) ;
#23274 = CIRCLE ( 'NONE', #687, 0.4692913385826771866 ) ;
#23275 = CARTESIAN_POINT ( 'NONE',  ( -0.3387265385688505437, -0.4407612517155324316, 0.9202755905511810219 ) ) ;
#23276 = CARTESIAN_POINT ( 'NONE',  ( 0.000000000000000000, 0.000000000000000000, 0.000000000000000000 ) ) ;
#23277 = CARTESIAN_POINT ( 'NONE',  ( -0.4173228346456693272, 5.110730736599190647E-17, -5.463696850393700654E-18 ) ) ;
#23278 = EDGE_CURVE ( 'NONE', #10521, #6256, #24439, .T. ) ;
#23279 = DIRECTION ( 'NONE',  ( 1.000000000000000000, 0.000000000000000000, 0.000000000000000000 ) ) ;
#23280 = CARTESIAN_POINT ( 'NONE',  ( 0.06200787401574806013, 0.000000000000000000, 0.7844728274238290666 ) ) ;
#23281 = CARTESIAN_POINT ( 'NONE',  ( 0.1522836969735573143, -0.1970374587079582740, -0.4531137400369409374 ) ) ;
#23282 = AXIS2_PLACEMENT_3D ( 'NONE', #4266, #25453, #19231 ) ;
#23283 = ORIENTED_EDGE ( 'NONE', *, *, #10512, .F. ) ;
#23284 = FACE_OUTER_BOUND ( 'NONE', #3939, .T. ) ;
#23285 = DIRECTION ( 'NONE',  ( 0.000000000000000000, 0.000000000000000000, 1.000000000000000000 ) ) ;
#23286 = B_SPLINE_CURVE_WITH_KNOTS ( 'NONE', 3,
 ( #11927, #1063, #20682, #22806, #22525, #15752, #5282, #18258 ),
 .UNSPECIFIED., .F., .F.,
 ( 4, 2, 2, 4 ),
 ( 0.000000000000000000, 0.1250000000000002220, 0.2500000000000002776, 0.5000000000000000000 ),
 .UNSPECIFIED. ) ;
#23287 = DIRECTION ( 'NONE',  ( 0.000000000000000000, 0.000000000000000000, 1.000000000000000000 ) ) ;
#23288 = EDGE_LOOP ( 'NONE', ( #14968, #5504, #24955, #3407, #11803, #18325 ) ) ;
#23289 = ORIENTED_EDGE ( 'NONE', *, *, #6214, .T. ) ;
#23290 = ORIENTED_EDGE ( 'NONE', *, *, #26449, .T. ) ;
#23291 = CARTESIAN_POINT ( 'NONE',  ( -0.03532354024591771724, -0.6299212598425196763, 0.000000000000000000 ) ) ;
#23292 = DIRECTION ( 'NONE',  ( 1.000000000000000000, 0.000000000000000000, 0.000000000000000000 ) ) ;
#23293 = CARTESIAN_POINT ( 'NONE',  ( -1.692913385826771533, 0.4724409448818898127, -1.036610629921259805E-16 ) ) ;
#23294 = CARTESIAN_POINT ( 'NONE',  ( -0.4954415918530867824, -0.1327036767659759697, 1.747047244094488194 ) ) ;
#23295 = ORIENTED_EDGE ( 'NONE', *, *, #440, .T. ) ;
#23296 = ORIENTED_EDGE ( 'NONE', *, *, #14142, .T. ) ;
#23297 = CARTESIAN_POINT ( 'NONE',  ( -0.3702005978258633423, 0.04877294052296513721, -3.115157480314960647 ) ) ;
#23298 = ORIENTED_EDGE ( 'NONE', *, *, #13512, .F. ) ;
#23299 = AXIS2_PLACEMENT_3D ( 'NONE', #24559, #7338, #11852 ) ;
#23300 = CARTESIAN_POINT ( 'NONE',  ( 0.1200170377978877767, -0.4465874321618642506, -1.928289503579156294 ) ) ;
#23301 = ( NAMED_UNIT ( * ) PLANE_ANGLE_UNIT ( ) SI_UNIT ( $, .RADIAN. ) ) ;
#23302 = EDGE_CURVE ( 'NONE', #24919, #1804, #17000, .T. ) ;
#23303 = LINE ( 'NONE', #3930, #14569 ) ;
#23304 = CARTESIAN_POINT ( 'NONE',  ( -0.2041304421298429650, -0.2660793235464223860, 1.973425196850393970 ) ) ;
#23305 = VERTEX_POINT ( 'NONE', #68 ) ;
#23306 = EDGE_LOOP ( 'NONE', ( #24566, #17766, #21380, #6022, #20046 ) ) ;
#23307 = CIRCLE ( 'NONE', #9256, 0.02755905511811023931 ) ;
#23308 = CARTESIAN_POINT ( 'NONE',  ( 0.4763861460130703329, 0.1275996891957705826, -1.550196850393700920 ) ) ;
#23309 = CARTESIAN_POINT ( 'NONE',  ( -0.03937007874015747977, 0.000000000000000000, 0.000000000000000000 ) ) ;
#23310 = LINE ( 'NONE', #23158, #23630 ) ;
#23311 = PRODUCT_RELATED_PRODUCT_CATEGORY ( 'part', '', ( #14568 ) ) ;
#23312 = ORIENTED_EDGE ( 'NONE', *, *, #25196, .F. ) ;
#23313 = EDGE_LOOP ( 'NONE', ( #6061, #7815, #14402, #10122, #16054, #24980 ) ) ;
#23314 = ORIENTED_EDGE ( 'NONE', *, *, #2233, .F. ) ;
#23315 = EDGE_CURVE ( 'NONE', #26561, #17373, #4897, .T. ) ;
#23316 = EDGE_CURVE ( 'NONE', #16472, #16219, #8519, .T. ) ;
#23317 = CARTESIAN_POINT ( 'NONE',  ( 0.07614184848677874040, -0.4941010236220472751, 6.050992370341708321E-17 ) ) ;
#23318 = DIRECTION ( 'NONE',  ( 0.000000000000000000, 1.000000000000000000, 0.000000000000000000 ) ) ;
#23319 = CARTESIAN_POINT ( 'NONE',  ( 0.3995939286813819935, -0.1970998888482827227, -1.934055118110237004 ) ) ;
#23320 = ORIENTED_EDGE ( 'NONE', *, *, #4372, .F. ) ;
#23321 = ORIENTED_EDGE ( 'NONE', *, *, #22466, .T. ) ;
#23322 = DIRECTION ( 'NONE',  ( 0.2036417511401759084, -0.4895227362422918116, -0.8478782506317885659 ) ) ;
#23323 = CONICAL_SURFACE ( 'NONE', #18766, 65.52281417845038902, 1.029744258088330700 ) ;
#23324 = DIRECTION ( 'NONE',  ( -0.000000000000000000, -0.000000000000000000, -1.000000000000000000 ) ) ;
#23325 = DIRECTION ( 'NONE',  ( 0.000000000000000000, 0.000000000000000000, 1.000000000000000000 ) ) ;
#23326 = DIRECTION ( 'NONE',  ( 0.000000000000000000, -1.000000000000000000, 0.000000000000000000 ) ) ;
#23327 = CIRCLE ( 'NONE', #12469, 0.1003956692913385990 ) ;
#23328 = CARTESIAN_POINT ( 'NONE',  ( -0.5719614286040570761, -0.2987169063169233807, 0.2011802169574927746 ) ) ;
#23329 = CARTESIAN_POINT ( 'NONE',  ( 0.2817828961649165298, 0.3666644560843322909, -1.928289503579156294 ) ) ;
#23330 = CARTESIAN_POINT ( 'NONE',  ( 0.009795313329799274632, -0.08526597544922021044, -0.4724409448841456749 ) ) ;
#23331 = CARTESIAN_POINT ( 'NONE',  ( -0.6069206441216355996, 1.114319256831733274, 0.05180297602608902041 ) ) ;
#23332 = DIRECTION ( 'NONE',  ( 0.000000000000000000, -1.000000000000000000, 0.000000000000000000 ) ) ;
#23333 = CARTESIAN_POINT ( 'NONE',  ( 0.4606299212598425341, 0.000000000000000000, 0.1771653543307086520 ) ) ;
#23334 = ORIENTED_EDGE ( 'NONE', *, *, #23097, .F. ) ;
#23335 = CARTESIAN_POINT ( 'NONE',  ( -0.2602238532265429005, 0.000000000000000000, -0.2362204724409449064 ) ) ;
#23336 = ORIENTED_EDGE ( 'NONE', *, *, #8618, .T. ) ;
#23337 = CARTESIAN_POINT ( 'NONE',  ( 0.3264619303874873313, -0.1888818218344748001, 0.07637630750536809898 ) ) ;
#23338 = DIRECTION ( 'NONE',  ( -1.000000000000000000, 0.000000000000000000, 0.000000000000000000 ) ) ;
#23339 = VERTEX_POINT ( 'NONE', #2137 ) ;
#23340 = CARTESIAN_POINT ( 'NONE',  ( 0.1714649452450068834, -0.4705186852026070898, 0.09684793308443542803 ) ) ;
#23341 = CARTESIAN_POINT ( 'NONE',  ( -0.7874015748031496509, -1.322410629921259858E-32, -0.6299212598425196763 ) ) ;
#23342 = VECTOR ( 'NONE', #12412, 39.37007874015748143 ) ;
#23343 = LINE ( 'NONE', #16397, #23866 ) ;
#23344 = CARTESIAN_POINT ( 'NONE',  ( -0.4382482975805018222, 0.3362148458988871713, 0.9202755905511811330 ) ) ;
#23345 = DIMENSIONAL_EXPONENTS ( 1.000000000000000000, 0.000000000000000000, 0.000000000000000000, 0.000000000000000000, 0.000000000000000000, 0.000000000000000000, 0.000000000000000000 ) ;
#23346 = ORIENTED_EDGE ( 'NONE', *, *, #21415, .F. ) ;
#23347 = EDGE_CURVE ( 'NONE', #10367, #2190, #23456, .T. ) ;
#23348 = LINE ( 'NONE', #27569, #918 ) ;
#23349 = ORIENTED_EDGE ( 'NONE', *, *, #19159, .T. ) ;
#23350 = PRESENTATION_STYLE_ASSIGNMENT (( #9902 ) ) ;
#23351 = EDGE_CURVE ( 'NONE', #13627, #7099, #9888, .T. ) ;
#23352 = CARTESIAN_POINT ( 'NONE',  ( 0.4537304931026565069, 0.07942646906837147469, 0.1903859678062056193 ) ) ;
#23353 = DIRECTION ( 'NONE',  ( 0.000000000000000000, 1.000000000000000000, 0.000000000000000000 ) ) ;
#23354 = DIRECTION ( 'NONE',  ( -0.000000000000000000, -1.000000000000000000, -0.000000000000000000 ) ) ;
#23355 = EDGE_LOOP ( 'NONE', ( #8351, #15891 ) ) ;
#23356 = CARTESIAN_POINT ( 'NONE',  ( -0.5905511811023621549, 1.087444635826771533, 0.1051828227901525498 ) ) ;
#23357 = ORIENTED_EDGE ( 'NONE', *, *, #15862, .F. ) ;
#23358 = CARTESIAN_POINT ( 'NONE',  ( 0.3007905576423843819, -0.1482986320106508549, 1.973425196850393970 ) ) ;
#23359 = CARTESIAN_POINT ( 'NONE',  ( 0.06699507805604380806, -0.5085118447796470598, -1.550196850393700920 ) ) ;
#23360 = DIRECTION ( 'NONE',  ( 0.5000000010362839475, 0.8660254031861397417, 0.000000000000000000 ) ) ;
#23361 = CARTESIAN_POINT ( 'NONE',  ( 0.009795313329799274632, -0.08526597544922021044, -0.4724409448841456749 ) ) ;
#23362 = CARTESIAN_POINT ( 'NONE',  ( -0.2262947209317479058, -0.4714317853999300256, 0.1392975274300493338 ) ) ;
#23363 = CARTESIAN_POINT ( 'NONE',  ( -0.4954197419817796266, -0.2442565704126152260, 0.9399606299212598381 ) ) ;
#23364 = CARTESIAN_POINT ( 'NONE',  ( 0.2089723435111824623, -0.4324731448915265508, 0.2362204724409445455 ) ) ;
#23365 = DIRECTION ( 'NONE',  ( -1.000000000000000000, 0.000000000000000000, 0.000000000000000000 ) ) ;
#23366 = ORIENTED_EDGE ( 'NONE', *, *, #12420, .F. ) ;
#23367 = B_SPLINE_SURFACE_WITH_KNOTS ( 'NONE', 2, 3, ( 
 ( #5036, #9259, #17875, #20292, #952, #3183, #11816, #27507, #16616, #6182, #27647, #18725, #22694, #10115, #5897, #1642, #8011, #12520, #11961, #10393, #20581, #3320, #18432, #1235, #27082, #23128, #3607, #16760, #3465, #16345, #8290, #9974, #1362, #14525, #20996, #10244, #14670, #24943, #25372, #19011, #12237, #5607, #6034, #18574, #20716, #3756, #14235, #18863, #27218, #22842, #12096, #7867, #16476, #23273, #25089, #3903, #21137, #1779, #16906, #5755, #14376, #22988, #20854, #1503, #27361, #12378 ),
 ( #10956, #2995, #2468, #6725, #13206, #382, #8829, #17453, #11093, #21834, #8561, #14942, #19715, #8964, #26068, #23554, #12927, #17587, #23419, #10533, #6311, #26200, #4187, #21551, #4461, #8423, #10817, #13075, #14810, #17178, #2197, #15361, #15076, #23689, #12796, #2059, #4050, #19433, #124, #4322, #6585, #25657, #12655, #21284, #21422, #15211, #27782, #23820, #21699, #1921, #23954, #17043, #19149, #10672, #19291, #25793, #6441, #2327, #19580, #259, #7129, #17971, #24086, #1065, #26336, #26608 ),
 ( #7405, #11639, #2866, #17714, #6860, #637, #7261, #17846, #13345, #9659, #22104, #13474, #779, #5135, #22381, #26751, #18260, #20261, #3154, #24356, #15487, #18106, #2733, #4859, #9367, #21970, #3003, #11365, #9095, #4722, #6999, #15622, #13762, #19981, #9506, #24625, #920, #16027, #24221, #2599, #9225, #26467, #15753, #5284, #15883, #4998, #11223, #13620, #22239, #11505, #20118, #24487, #13908, #22527, #14052, #5439, #16176, #20547, #24773, #22665, #1204, #26896, #3290, #11929, #9804, #7547 ) ),
 .UNSPECIFIED., .F., .T., .F.,
 ( 3, 3 ),
 ( 4, 2, 2, 2, 2, 2, 2, 2, 2, 2, 2, 2, 2, 2, 2, 2, 2, 2, 2, 2, 2, 2, 2, 2, 2, 2, 2, 2, 2, 2, 2, 2, 4 ),
 ( 0.000000000000000000, 1.000000000000000000 ),
 ( 0.000000000000000000, 0.1963495408493620697, 0.3926990816987241395, 0.5890486225480862092, 0.7853981633974482790, 0.9817477042468103487, 1.178097245096172418, 1.374446785945534488, 1.570796326794896558, 1.767145867644258628, 1.963495408493620697, 2.159844949342982545, 2.356194490192344837, 2.552544031041707129, 2.748893571891068976, 2.945243112740430824, 3.141592653589793116, 3.337942194439155408, 3.534291735288517255, 3.730641276137879103, 3.926990816987241395, 4.123340357836603687, 4.319689898685965090, 4.516039439535327382, 4.712388980384689674, 4.908738521234051966, 5.105088062083414258, 5.301437602932775661, 5.497787143782137953, 5.694136684631500245, 5.890486225480861648, 6.086835766330223940, 6.283185307179586232 ),
 .UNSPECIFIED. ) ;
#23368 = CARTESIAN_POINT ( 'NONE',  ( -0.2842163005027485978, 0.2181214148711163314, -3.115157480314960203 ) ) ;
#23369 = VERTEX_POINT ( 'NONE', #15013 ) ;
#23370 = EDGE_CURVE ( 'NONE', #14826, #3213, #11902, .T. ) ;
#23371 = CARTESIAN_POINT ( 'NONE',  ( -0.4301570366550043767, -0.3771675965699594624, 0.9399606299212597271 ) ) ;
#23372 = FACE_BOUND ( 'NONE', #17893, .T. ) ;
#23373 = CARTESIAN_POINT ( 'NONE',  ( 0.000000000000000000, 0.07874015746264864668, 0.000000000000000000 ) ) ;
#23374 = ADVANCED_FACE ( 'NONE', ( #17390 ), #26979, .T. ) ;
#23375 = CARTESIAN_POINT ( 'NONE',  ( -0.5811915241081616612, -0.4724399524670138684, 0.9954595399565421276 ) ) ;
#23376 = EDGE_LOOP ( 'NONE', ( #15957, #7408 ) ) ;
#23377 = CIRCLE ( 'NONE', #11167, 0.01377952755905510404 ) ;
#23378 = CARTESIAN_POINT ( 'NONE',  ( -0.1771653543307086520, 0.1673228346456692994, 0.000000000000000000 ) ) ;
#23379 = CARTESIAN_POINT ( 'NONE',  ( -0.5744830435817726011, -0.4891464190265612522, -0.9948699164926496641 ) ) ;
#23380 = CIRCLE ( 'NONE', #11605, 1.377952755905512472 ) ;
#23381 = DIRECTION ( 'NONE',  ( 0.000000000000000000, 0.000000000000000000, 1.000000000000000000 ) ) ;
#23382 = CARTESIAN_POINT ( 'NONE',  ( -0.3432721300506699214, 0.06002180498064106640, 0.1166443193921996718 ) ) ;
#23383 = DIRECTION ( 'NONE',  ( 0.000000000000000000, 0.000000000000000000, 1.000000000000000000 ) ) ;
#23384 = ORIENTED_EDGE ( 'NONE', *, *, #24999, .F. ) ;
#23385 = CARTESIAN_POINT ( 'NONE',  ( -0.2128972891168988413, -0.5836425148029299459, 0.2574819594177527593 ) ) ;
#23386 = CARTESIAN_POINT ( 'NONE',  ( 0.1495939273659966928, 0.4806208190371651368, 0.02345246241340225024 ) ) ;
#23387 = VERTEX_POINT ( 'NONE', #9038 ) ;
#23388 = EDGE_CURVE ( 'NONE', #27836, #12685, #844, .T. ) ;
#23389 = CARTESIAN_POINT ( 'NONE',  ( 0.1173917140416396443, 0.4382752542996237732, -1.934055118110236338 ) ) ;
#23390 = CIRCLE ( 'NONE', #5841, 0.5118110236220472231 ) ;
#23391 = ORIENTED_EDGE ( 'NONE', *, *, #11166, .F. ) ;
#23392 = ORIENTED_EDGE ( 'NONE', *, *, #12085, .F. ) ;
#23393 = MECHANICAL_DESIGN_GEOMETRIC_PRESENTATION_REPRESENTATION (  '', ( #16571 ), #8499 ) ;
#23394 = CARTESIAN_POINT ( 'NONE',  ( -0.5252801253069795395, -0.4673450799357756202, 0.1486916858744336545 ) ) ;
#23395 = SURFACE_STYLE_USAGE ( .BOTH. , #1899 ) ;
#23396 = EDGE_LOOP ( 'NONE', ( #13248, #841, #13784, #24499 ) ) ;
#23397 = EDGE_CURVE ( 'NONE', #27022, #3924, #18160, .T. ) ;
#23398 = CARTESIAN_POINT ( 'NONE',  ( -0.1599629598573824862, -0.4411872753631803090, 0.07637795275590551769 ) ) ;
#23399 = CARTESIAN_POINT ( 'NONE',  ( -0.6169740991250696194, -0.4807978361619021923, 0.9954634121926729806 ) ) ;
#23401 = CARTESIAN_POINT ( 'NONE',  ( 0.4932821129636645874, 0.08637579872942321990, 0.2574803149606298969 ) ) ;
#23400 = TOROIDAL_SURFACE ( 'NONE', #11195, 0.4055118110236220486, 0.01181102362204724393 ) ;
#23402 = B_SPLINE_CURVE_WITH_KNOTS ( 'NONE', 3,
 ( #13918, #22389, #27056, #26475, #7706, #24364, #13626, #24493, #3010, #11648, #5445, #927, #14058 ),
 .UNSPECIFIED., .F., .F.,
 ( 4, 1, 1, 1, 1, 1, 1, 1, 1, 1, 4 ),
 ( 0.3833360769390280476, 0.3893635454205919832, 0.3944867497131970269, 0.4047331582984080023, 0.4098563625910129904, 0.4201027711762239658, 0.4252259754688289539, 0.4405955883466449730, 0.4508419969318550047, 0.4713348141022760118, 0.4911627496483090272 ),
 .UNSPECIFIED. ) ;
#23403 = CARTESIAN_POINT ( 'NONE',  ( 0.2208527687061731248, -0.6048181665932198525, 0.1183902030356892010 ) ) ;
#23404 = EDGE_CURVE ( 'NONE', #12651, #25917, #15954, .T. ) ;
#23405 = VERTEX_POINT ( 'NONE', #10606 ) ;
#23406 = CARTESIAN_POINT ( 'NONE',  ( 0.3543307086614173596, 0.000000000000000000, 1.953740157480315043 ) ) ;
#23407 = VERTEX_POINT ( 'NONE', #449 ) ;
#23408 = ORIENTED_EDGE ( 'NONE', *, *, #10333, .F. ) ;
#23409 = CARTESIAN_POINT ( 'NONE',  ( -0.6254176984700635655, -0.07018457039985938339, -0.2392426808639660785 ) ) ;
#23410 = LINE ( 'NONE', #8144, #14781 ) ;
#23411 = CARTESIAN_POINT ( 'NONE',  ( 0.4067073728345788064, -0.2341441294389338956, 0.1992125984251968684 ) ) ;
#23412 = CARTESIAN_POINT ( 'NONE',  ( -0.5177165354330708347, 0.9448818897637796255, -9.561468503937007847E-18 ) ) ;
#23413 = EDGE_LOOP ( 'NONE', ( #24183, #20454 ) ) ;
#23414 = VERTEX_POINT ( 'NONE', #2402 ) ;
#23415 = DIRECTION ( 'NONE',  ( -0.000000000000000000, 1.000000000000000000, -0.000000000000000000 ) ) ;
#23416 = CARTESIAN_POINT ( 'NONE',  ( -0.09842519685039370636, -5.111401574803149519E-18, 0.000000000000000000 ) ) ;
#23417 = CONICAL_SURFACE ( 'NONE', #11661, 0.6102362204724409711, 0.7853981625000032718 ) ;
#23418 = CONICAL_SURFACE ( 'NONE', #10293, 0.5511811023975373702, 0.7853981633974482790 ) ;
#23419 = CARTESIAN_POINT ( 'NONE',  ( 0.04877294052295595012, 0.3702005978258479102, -3.115157480314960647 ) ) ;
#23420 = CARTESIAN_POINT ( 'NONE',  ( -0.06200787401574775481, 7.593774443531783063E-18, -4.330708661417323135 ) ) ;
#23421 = FILL_AREA_STYLE_COLOUR ( '', #17486 ) ;
#23422 = DIRECTION ( 'NONE',  ( 0.000000000000000000, 0.000000000000000000, -1.000000000000000000 ) ) ;
#23423 = DIRECTION ( 'NONE',  ( 0.000000000000000000, 0.000000000000000000, -1.000000000000000000 ) ) ;
#23424 = DIRECTION ( 'NONE',  ( 1.000000000000000000, 0.000000000000000000, 0.000000000000000000 ) ) ;
#23426 = CARTESIAN_POINT ( 'NONE',  ( -0.5511811023622047445, 0.03607471876259063515, 0.9202755905511811330 ) ) ;
#23425 = CIRCLE ( 'NONE', #27012, 0.07677362204724409722 ) ;
#23427 = ORIENTED_EDGE ( 'NONE', *, *, #18095, .F. ) ;
#23428 = DIRECTION ( 'NONE',  ( 0.7660444431189775694, -0.6427876096865398070, 0.000000000000000000 ) ) ;
#23429 = DIRECTION ( 'NONE',  ( -1.224646799147353207E-16, 1.000000000000000000, 0.000000000000000000 ) ) ;
#23430 = DIRECTION ( 'NONE',  ( 1.000000000000000000, 0.000000000000000000, 0.000000000000000000 ) ) ;
#23431 = SHAPE_DEFINITION_REPRESENTATION ( #7770, #5415 ) ;
#23432 = CARTESIAN_POINT ( 'NONE',  ( -0.5085118447801421082, 0.06699507805369804558, 1.766732283464566899 ) ) ;
#23433 = CIRCLE ( 'NONE', #22498, 0.3937007874015748254 ) ;
#23434 = ORIENTED_EDGE ( 'NONE', *, *, #16544, .F. ) ;
#23435 = ORIENTED_EDGE ( 'NONE', *, *, #1186, .T. ) ;
#23436 = CIRCLE ( 'NONE', #23871, 0.3937007874015748254 ) ;
#23437 = CARTESIAN_POINT ( 'NONE',  ( -0.09269288654273742656, -0.3460635936745020680, -3.115157480314960647 ) ) ;
#23438 = ORIENTED_EDGE ( 'NONE', *, *, #23172, .T. ) ;
#23439 = CARTESIAN_POINT ( 'NONE',  ( -0.09842519685039370636, 0.07874015748031495954, -0.04546065111729338803 ) ) ;
#23440 = CIRCLE ( 'NONE', #15755, 0.6881889763779527325 ) ;
#23441 = CARTESIAN_POINT ( 'NONE',  ( 3.387491338582676985E-16, -0.6299212598425196763, 0.000000000000000000 ) ) ;
#23442 = ( CONVERSION_BASED_UNIT ( 'INCH', #15102 ) LENGTH_UNIT ( ) NAMED_UNIT ( #7220 ) ) ;
#23443 = CARTESIAN_POINT ( 'NONE',  ( 0.000000000000000000, 0.000000000000000000, 0.1377952755905511861 ) ) ;
#23444 = EDGE_CURVE ( 'NONE', #27804, #23052, #13227, .T. ) ;
#23445 = CARTESIAN_POINT ( 'NONE',  ( -0.3346456692913385988, -0.02190250779246036283, 1.973425196850393970 ) ) ;
#23446 = VERTEX_POINT ( 'NONE', #11032 ) ;
#23447 = VERTEX_POINT ( 'NONE', #4794 ) ;
#23448 = CARTESIAN_POINT ( 'NONE',  ( 0.3912931228432187658, 0.3001918266902420251, -1.550196850393700920 ) ) ;
#23449 = CARTESIAN_POINT ( 'NONE',  ( -0.09842519685039370636, 5.809059055118109875E-18, -0.09092130223458683158 ) ) ;
#23450 = CARTESIAN_POINT ( 'NONE',  ( 0.5981657849660177995, -0.2403521948818897747, 0.4163022132461299263 ) ) ;
#23451 = CIRCLE ( 'NONE', #23901, 0.3149606299212598381 ) ;
#23452 = EDGE_LOOP ( 'NONE', ( #20424, #5927, #20069, #22754 ) ) ;
#23453 = ORIENTED_EDGE ( 'NONE', *, *, #12450, .T. ) ;
#23454 = FACE_OUTER_BOUND ( 'NONE', #25554, .T. ) ;
#23455 = B_SPLINE_CURVE_WITH_KNOTS ( 'NONE', 3,
 ( #4765, #543, #9139, #21741, #2368, #6492, #11000, #21878 ),
 .UNSPECIFIED., .F., .F.,
 ( 4, 2, 2, 4 ),
 ( 0.000000000000000000, 0.1250000000000001110, 0.2500000000000002220, 0.5000000000000000000 ),
 .UNSPECIFIED. ) ;
#23456 = CIRCLE ( 'NONE', #27041, 0.3771653543307086909 ) ;
#23457 = LINE ( 'NONE', #23317, #21664 ) ;
#23458 = CARTESIAN_POINT ( 'NONE',  ( -0.09842519685039387289, 0.2991866959364304357, -3.554781501636282037 ) ) ;
#23459 = PLANE ( 'NONE',  #20956 ) ;
#23460 = ORIENTED_EDGE ( 'NONE', *, *, #21081, .T. ) ;
#23461 = VECTOR ( 'NONE', #4564, 39.37007874015748143 ) ;
#23462 = CARTESIAN_POINT ( 'NONE',  ( 0.3149606299212598381, 3.857155272905049219E-17, -0.4448818897637791814 ) ) ;
#23463 = CIRCLE ( 'NONE', #14895, 0.6212598425196850238 ) ;
#23464 = CARTESIAN_POINT ( 'NONE',  ( 0.000000000000000000, 0.5007874015748031704, 0.3543307086614173040 ) ) ;
#23465 = ADVANCED_FACE ( 'NONE', ( #17119, #2542 ), #11164, .T. ) ;
#23466 = DIRECTION ( 'NONE',  ( 1.000000000000000078E-15, -1.000000000000000000, 0.000000000000000000 ) ) ;
#23467 = CARTESIAN_POINT ( 'NONE',  ( -0.5144115741929539132, -0.5069565267453091106, 0.1348810065547058623 ) ) ;
#23468 = LINE ( 'NONE', #14852, #7172 ) ;
#23469 = CARTESIAN_POINT ( 'NONE',  ( -0.6075516362842373619, 1.113574658101797121, 0.05417226358486029736 ) ) ;
#23470 = FACE_OUTER_BOUND ( 'NONE', #6643, .T. ) ;
#23471 = CARTESIAN_POINT ( 'NONE',  ( 0.07874015747999522918, 0.1968503937007873850, -3.262328874726532213 ) ) ;
#23472 = DIRECTION ( 'NONE',  ( 0.000000000000000000, 0.000000000000000000, -1.000000000000000000 ) ) ;
#23473 = VERTEX_POINT ( 'NONE', #12869 ) ;
#23474 = EDGE_CURVE ( 'NONE', #18994, #22878, #24562, .T. ) ;
#23475 = VERTEX_POINT ( 'NONE', #26406 ) ;
#23476 = DIRECTION ( 'NONE',  ( 1.000000000000000000, 0.000000000000000000, 0.000000000000000000 ) ) ;
#23477 = CIRCLE ( 'NONE', #15786, 0.5905511811023621549 ) ;
#23478 = ORIENTED_EDGE ( 'NONE', *, *, #19902, .F. ) ;
#23479 = AXIS2_PLACEMENT_3D ( 'NONE', #21533, #6697, #17690 ) ;
#23480 = CARTESIAN_POINT ( 'NONE',  ( 0.3905379133858267737, -0.2805118110236220486, -0.4858607088160724063 ) ) ;
#23481 = CARTESIAN_POINT ( 'NONE',  ( -0.3882259019063066807, 0.3087756353526792119, 0.1734435147361200746 ) ) ;
#23482 = CARTESIAN_POINT ( 'NONE',  ( 0.5476281405333177643, 0.07214854559198216610, 0.9202755905511811330 ) ) ;
#23483 = ORIENTED_EDGE ( 'NONE', *, *, #5518, .F. ) ;
#23484 = CARTESIAN_POINT ( 'NONE',  ( 3.874463478174096549E-17, -1.533249767903113305E-16, 0.3163739521363750362 ) ) ;
#23485 = ORIENTED_EDGE ( 'NONE', *, *, #22135, .F. ) ;
#23486 = AXIS2_PLACEMENT_3D ( 'NONE', #13132, #10743, #17242 ) ;
#23487 = CARTESIAN_POINT ( 'NONE',  ( -0.4980314960629921295, 0.000000000000000000, -0.2618110236220472231 ) ) ;
#23488 = CARTESIAN_POINT ( 'NONE',  ( 0.03008364706454716778, 0.2273032555864669124, 9.010881889763779798E-17 ) ) ;
#23489 = EDGE_CURVE ( 'NONE', #24104, #21708, #19345, .T. ) ;
#23490 = EDGE_LOOP ( 'NONE', ( #10498, #903 ) ) ;
#23491 = CARTESIAN_POINT ( 'NONE',  ( 0.000000000000000000, 0.000000000000000000, 1.707677165389662743 ) ) ;
#23492 = CARTESIAN_POINT ( 'NONE',  ( 0.2350342994840594057, 0.2808987121547457666, 0.1910323753025394145 ) ) ;
#23493 = ORIENTED_EDGE ( 'NONE', *, *, #26022, .T. ) ;
#23494 = DIRECTION ( 'NONE',  ( 1.000000000000000000, 0.000000000000000000, 0.000000000000000000 ) ) ;
#23495 = AXIS2_PLACEMENT_3D ( 'NONE', #12479, #6410, #23517 ) ;
#23496 = DIRECTION ( 'NONE',  ( 0.000000000000000000, 0.000000000000000000, -1.000000000000000000 ) ) ;
#23497 = AXIS2_PLACEMENT_3D ( 'NONE', #3798, #1677, #16944 ) ;
#23498 = CARTESIAN_POINT ( 'NONE',  ( 0.5335524835332415838, 0.1429116519061139345, 0.9399606299212598381 ) ) ;
#23499 = DIRECTION ( 'NONE',  ( -0.9575713608335526539, 0.2881962680386024878, 1.067350012615773080E-17 ) ) ;
#23500 = EDGE_LOOP ( 'NONE', ( #25709, #27212, #4815, #24225 ) ) ;
#23501 = CARTESIAN_POINT ( 'NONE',  ( 0.3460502918090235247, 0.09275248786873148410, -3.115157480314960203 ) ) ;
#23502 = EDGE_CURVE ( 'NONE', #11259, #22433, #15620, .T. ) ;
#23503 = CARTESIAN_POINT ( 'NONE',  ( 0.5241918773311228241, 6.503874318720813848E-17, -0.2204724409448818867 ) ) ;
#23504 = AXIS2_PLACEMENT_3D ( 'NONE', #7156, #20573, #1227 ) ;
#23505 = ADVANCED_FACE ( 'NONE', ( #2945 ), #22175, .T. ) ;
#23506 = ORIENTED_EDGE ( 'NONE', *, *, #8946, .T. ) ;
#23507 = CARTESIAN_POINT ( 'NONE',  ( 0.2268096725200263730, 0.4600326175569572351, -1.550196850393700920 ) ) ;
#23508 = EDGE_LOOP ( 'NONE', ( #3571, #4415, #18092, #18203, #20557, #10738 ) ) ;
#23509 = CARTESIAN_POINT ( 'NONE',  ( 0.5417516942598733509, -0.1838445375782305768, 0.9399606299212601712 ) ) ;
#23510 = CARTESIAN_POINT ( 'NONE',  ( 0.1196556571321023277, -0.3272932875281243104, 0.1589462317991687523 ) ) ;
#23511 = CARTESIAN_POINT ( 'NONE',  ( -0.1180276236025431108, -0.3257325899126712887, 0.1478915661198716980 ) ) ;
#23512 = PLANE ( 'NONE',  #19066 ) ;
#23513 = CARTESIAN_POINT ( 'NONE',  ( -1.692913385826771533, 0.4724409448818898127, 0.1181102362204718981 ) ) ;
#23514 = ORIENTED_EDGE ( 'NONE', *, *, #18293, .T. ) ;
#23515 = CYLINDRICAL_SURFACE ( 'NONE', #15761, 0.3937007874015748254 ) ;
#23516 = VECTOR ( 'NONE', #664, 39.37007874015748143 ) ;
#23517 = DIRECTION ( 'NONE',  ( -1.000000000000000000, 0.000000000000000000, 0.000000000000000000 ) ) ;
#23518 = CARTESIAN_POINT ( 'NONE',  ( 0.4246272423004305296, 0.5071139714523401620, 0.1616495878881752113 ) ) ;
#23519 = LINE ( 'NONE', #25484, #7266 ) ;
#23520 = VERTEX_POINT ( 'NONE', #20337 ) ;
#23521 = FACE_OUTER_BOUND ( 'NONE', #16416, .T. ) ;
#23522 = AXIS2_PLACEMENT_3D ( 'NONE', #24098, #13216, #22115 ) ;
#23523 = DIRECTION ( 'NONE',  ( -1.000000000000000000, 0.000000000000000000, 0.000000000000000000 ) ) ;
#23524 = PRODUCT_DEFINITION_CONTEXT ( 'detailed design', #21371, 'design' ) ;
#23525 = CARTESIAN_POINT ( 'NONE',  ( 0.2006393256663384084, 0.4069519308876483610, -1.934055118110236338 ) ) ;
#23526 = ADVANCED_FACE ( 'NONE', ( #708 ), #9582, .T. ) ;
#23527 = ADVANCED_FACE ( 'NONE', ( #4939, #20192 ), #13556, .T. ) ;
#23528 = B_SPLINE_CURVE_WITH_KNOTS ( 'NONE', 3,
 ( #12645, #21272, #19138, #27770, #17033, #8411 ),
 .UNSPECIFIED., .F., .F.,
 ( 4, 2, 4 ),
 ( 0.000000000000000000, 0.5000000000000000000, 1.000000000000000000 ),
 .UNSPECIFIED. ) ;
#23529 = AXIS2_PLACEMENT_3D ( 'NONE', #8558, #17177, #25791 ) ;
#23530 = ORIENTED_EDGE ( 'NONE', *, *, #9257, .T. ) ;
#23531 = VERTEX_POINT ( 'NONE', #11855 ) ;
#23532 = CARTESIAN_POINT ( 'NONE',  ( -0.4769977115679039370, -0.6478166167414666221, 0.06212561209344763524 ) ) ;
#23533 = SURFACE_SIDE_STYLE ('',( #6566 ) ) ;
#23534 = CARTESIAN_POINT ( 'NONE',  ( 0.000000000000000000, 0.000000000000000000, -0.1309055118110236116 ) ) ;
#23535 = EDGE_LOOP ( 'NONE', ( #14451, #15011 ) ) ;
#23536 = EDGE_CURVE ( 'NONE', #20290, #10134, #20001, .T. ) ;
#23537 = COLOUR_RGB ( '', 0.40784314, 0.44705882, 0.49803922) ;
#23538 = VECTOR ( 'NONE', #19007, 39.37007874015748143 ) ;
#23539 = CARTESIAN_POINT ( 'NONE',  ( 0.5949363243629232079, -0.1357903337134992172, 0.1062972440944881941 ) ) ;
#23540 = FACE_OUTER_BOUND ( 'NONE', #16840, .T. ) ;
#23541 = CARTESIAN_POINT ( 'NONE',  ( 0.000000000000000000, 0.3937007873309092409, -2.066929133858267598 ) ) ;
#23542 = ORIENTED_EDGE ( 'NONE', *, *, #11034, .F. ) ;
#23543 = CARTESIAN_POINT ( 'NONE',  ( -0.1570220809524473238, 0.3184841198566425446, 1.953740157480315043 ) ) ;
#23544 = EDGE_CURVE ( 'NONE', #6246, #2628, #6540, .T. ) ;
#23545 = EDGE_LOOP ( 'NONE', ( #16779, #8640, #18746, #19353 ) ) ;
#23546 = CARTESIAN_POINT ( 'NONE',  ( -0.6222485084499363994, -0.07732954745974893185, -0.2398894390934003529 ) ) ;
#23547 = DIRECTION ( 'NONE',  ( 0.000000000000000000, 0.000000000000000000, 1.000000000000000000 ) ) ;
#23548 = CARTESIAN_POINT ( 'NONE',  ( -0.2860899518037610667, -0.4954156765914530247, 0.9399606299212598381 ) ) ;
#23549 = DIRECTION ( 'NONE',  ( 0.000000000000000000, 1.000000000000000000, 0.000000000000000000 ) ) ;
#23550 = CARTESIAN_POINT ( 'NONE',  ( 0.000000000000000000, 0.000000000000000000, -1.550196850393700920 ) ) ;
#23551 = CARTESIAN_POINT ( 'NONE',  ( 0.000000000000000000, 0.000000000000000000, 0.2574803149606298969 ) ) ;
#23552 = FACE_OUTER_BOUND ( 'NONE', #24008, .T. ) ;
#23553 = CIRCLE ( 'NONE', #8195, 0.3937007874015748254 ) ;
#23554 = CARTESIAN_POINT ( 'NONE',  ( -0.04877294052296160531, 0.3702005978258477437, -3.115157480314960647 ) ) ;
#23555 = DIRECTION ( 'NONE',  ( 0.000000000000000000, 0.000000000000000000, 1.000000000000000000 ) ) ;
#23556 = CARTESIAN_POINT ( 'NONE',  ( -0.3606190329934327310, 0.4297690281277732338, 0.1771653543307086520 ) ) ;
#23557 = DIRECTION ( 'NONE',  ( 0.000000000000000000, 1.000000000000000000, 0.000000000000000000 ) ) ;
#23558 = CARTESIAN_POINT ( 'NONE',  ( 0.000000000000000000, 0.07874015748031495954, -1.692913385826771533 ) ) ;
#23559 = DIRECTION ( 'NONE',  ( 0.000000000000000000, 0.000000000000000000, -1.000000000000000000 ) ) ;
#23560 = ADVANCED_FACE ( 'NONE', ( #16107, #573 ), #24699, .T. ) ;
#23561 = VECTOR ( 'NONE', #6426, 39.37007874015748143 ) ;
#23562 = CARTESIAN_POINT ( 'NONE',  ( -0.7217751814648617481, -0.1639319465211148685, 0.2562996995908388698 ) ) ;
#23563 = EDGE_CURVE ( 'NONE', #15096, #1388, #12791, .T. ) ;
#23564 = EDGE_LOOP ( 'NONE', ( #828, #6484, #4275, #26775 ) ) ;
#23565 = CARTESIAN_POINT ( 'NONE',  ( 0.5383630292499967940, 0.4286833100733393742, 0.1322818203437346463 ) ) ;
#23566 = ORIENTED_EDGE ( 'NONE', *, *, #11576, .T. ) ;
#23567 = CARTESIAN_POINT ( 'NONE',  ( -0.3041553300245939950, 0.05901566860999998831, -0.2362204724409447953 ) ) ;
#23568 = CARTESIAN_POINT ( 'NONE',  ( 0.1522836969735573143, 0.2938892803217901806, -0.3971963147566898167 ) ) ;
#23569 = CARTESIAN_POINT ( 'NONE',  ( -0.1327036767659680594, 0.4954415918530845619, 1.766732283464566899 ) ) ;
#23570 = EDGE_CURVE ( 'NONE', #24185, #14002, #24061, .T. ) ;
#23571 = CARTESIAN_POINT ( 'NONE',  ( -0.3855916753051397139, 0.3382184156732160329, 1.747047244094488194 ) ) ;
#23572 = EDGE_LOOP ( 'NONE', ( #15345, #12226, #7882, #11045, #22827, #19495, #7985 ) ) ;
#23573 = AXIS2_PLACEMENT_3D ( 'NONE', #6826, #15453, #25899 ) ;
#23574 = ORIENTED_EDGE ( 'NONE', *, *, #4185, .T. ) ;
#23575 = CARTESIAN_POINT ( 'NONE',  ( 0.09269288654274054906, 0.3460635936744927976, -3.115157480314960647 ) ) ;
#23576 = VERTEX_POINT ( 'NONE', #27404 ) ;
#23577 = CARTESIAN_POINT ( 'NONE',  ( -0.3998447049182496382, 0.4754871227240771714, 0.09685039370078740717 ) ) ;
#23578 = ORIENTED_EDGE ( 'NONE', *, *, #3674, .F. ) ;
#23579 = FACE_OUTER_BOUND ( 'NONE', #6640, .T. ) ;
#23580 = CARTESIAN_POINT ( 'NONE',  ( 0.2660793235464301021, -0.2041304421298313909, 1.973425196850393970 ) ) ;
#23581 = ADVANCED_FACE ( 'NONE', ( #10288, #6080 ), #1825, .T. ) ;
#23582 = ORIENTED_EDGE ( 'NONE', *, *, #6894, .T. ) ;
#23583 = ORIENTED_EDGE ( 'NONE', *, *, #22966, .T. ) ;
#23584 = CIRCLE ( 'NONE', #9558, 0.3346456692913385988 ) ;
#23585 = CARTESIAN_POINT ( 'NONE',  ( 0.4270824798167666692, -0.2466292688015215839, -1.550196850393700920 ) ) ;
#23586 = FACE_OUTER_BOUND ( 'NONE', #14610, .T. ) ;
#23587 = VERTEX_POINT ( 'NONE', #22733 ) ;
#23588 = ORIENTED_EDGE ( 'NONE', *, *, #24698, .T. ) ;
#23589 = ORIENTED_EDGE ( 'NONE', *, *, #13165, .T. ) ;
#23590 = DIRECTION ( 'NONE',  ( 0.000000000000000000, 1.000000000000000000, 0.000000000000000000 ) ) ;
#23591 = CYLINDRICAL_SURFACE ( 'NONE', #22560, 0.3937007874015748254 ) ;
#23592 = DIRECTION ( 'NONE',  ( 0.000000000000000000, 0.000000000000000000, 1.000000000000000000 ) ) ;
#23593 = CARTESIAN_POINT ( 'NONE',  ( 0.4714076450716228051, 0.08371568475168257584, 0.1920935997044048160 ) ) ;
#23594 = ORIENTED_EDGE ( 'NONE', *, *, #26948, .T. ) ;
#23595 = B_SPLINE_SURFACE_WITH_KNOTS ( 'NONE', 3, 3, ( 
 ( #19885, #7030, #15915, #2765, #7296, #18142 ),
 ( #26786, #537, #16063, #5170, #22555, #15783 ),
 ( #9128, #24522, #17747, #22272, #26369, #5466 ),
 ( #9694, #3037, #11533, #7579, #11671, #16206 ) ),
 .UNSPECIFIED., .F., .F., .F.,
 ( 4, 4 ),
 ( 4, 1, 1, 4 ),
 ( -1.199999999999999956, 0.000000000000000000 ),
 ( -3.749855894370895282, -2.141060511069079908, -1.068530255534539952, 0.004000000000000000083 ),
 .UNSPECIFIED. ) ;
#23596 = EDGE_CURVE ( 'NONE', #17618, #8482, #10081, .T. ) ;
#23597 = TOROIDAL_SURFACE ( 'NONE', #5525, 0.4232283464566928832, 0.07677165354330708902 ) ;
#23598 = CARTESIAN_POINT ( 'NONE',  ( 0.000000000000000000, 0.000000000000000000, 0.1377952755905511861 ) ) ;
#23599 = CARTESIAN_POINT ( 'NONE',  ( 0.2362204724225640262, 0.000000000000000000, -4.330708661417323135 ) ) ;
#23600 = AXIS2_PLACEMENT_3D ( 'NONE', #9147, #17767, #11415 ) ;
#23601 = EDGE_CURVE ( 'NONE', #1745, #22507, #23641, .T. ) ;
#23602 = DIRECTION ( 'NONE',  ( 0.000000000000000000, -1.000000000000000000, 0.000000000000000000 ) ) ;
#23603 = CARTESIAN_POINT ( 'NONE',  ( 0.9842519685039370358, 1.801181102362204633, 0.2952755905511810774 ) ) ;
#23604 = EDGE_CURVE ( 'NONE', #1421, #11291, #23057, .T. ) ;
#23605 = CARTESIAN_POINT ( 'NONE',  ( 0.4921259842519686289, 0.06441914069860960046, -1.569881889763779625 ) ) ;
#23606 = CARTESIAN_POINT ( 'NONE',  ( -0.0001974756197917525776, 0.5007874015748032814, 0.2574827755769819038 ) ) ;
#23607 = CARTESIAN_POINT ( 'NONE',  ( 0.04956879678463937261, 0.1968503937007873850, -3.186635197791150453 ) ) ;
#23608 = VERTEX_POINT ( 'NONE', #27549 ) ;
#23609 = CARTESIAN_POINT ( 'NONE',  ( 0.1580799066051618851, -0.4326553680327471785, 0.1771653543307085410 ) ) ;
#23610 = B_SPLINE_CURVE_WITH_KNOTS ( 'NONE', 3,
 ( #5537, #16540, #14161, #12457 ),
 .UNSPECIFIED., .F., .F.,
 ( 4, 4 ),
 ( 0.000000000000000000, 0.0001798248967499302582 ),
 .UNSPECIFIED. ) ;
#23611 = CIRCLE ( 'NONE', #3719, 0.1298643763538142593 ) ;
#23612 = ORIENTED_EDGE ( 'NONE', *, *, #15985, .T. ) ;
#23613 = CIRCLE ( 'NONE', #18124, 0.1476377952755905387 ) ;
#23614 = CARTESIAN_POINT ( 'NONE',  ( -0.4067073728345488304, -0.2341441294389850492, 0.07637795275590551769 ) ) ;
#23615 = LINE ( 'NONE', #2528, #3516 ) ;
#23616 = ORIENTED_EDGE ( 'NONE', *, *, #21914, .T. ) ;
#23617 = CARTESIAN_POINT ( 'NONE',  ( 0.000000000000000000, 0.6881889763779527325, 0.4724409448818898127 ) ) ;
#23618 = EDGE_LOOP ( 'NONE', ( #15776, #24107, #1810, #22397 ) ) ;
#23619 = EDGE_CURVE ( 'NONE', #798, #9216, #6935, .T. ) ;
#23620 = CARTESIAN_POINT ( 'NONE',  ( -0.5525004126151165096, 0.09742072959660473541, 0.2775610236220472093 ) ) ;
#23621 = AXIS2_PLACEMENT_3D ( 'NONE', #5218, #3362, #18482 ) ;
#23622 = DIRECTION ( 'NONE',  ( 0.5518027697606309179, -6.757634957480006187E-17, 0.8339746418713797071 ) ) ;
#23623 = DIRECTION ( 'NONE',  ( 1.000000000000000000, 0.000000000000000000, 0.000000000000000000 ) ) ;
#23624 = DIRECTION ( 'NONE',  ( -1.000000000000000000, 0.000000000000000000, 0.000000000000000000 ) ) ;
#23625 = ORIENTED_EDGE ( 'NONE', *, *, #12749, .T. ) ;
#23626 = CARTESIAN_POINT ( 'NONE',  ( 0.6707652279343464530, -0.1538768215239712522, 0.1322834645669291320 ) ) ;
#23627 = DIRECTION ( 'NONE',  ( 0.000000000000000000, 0.000000000000000000, -1.000000000000000000 ) ) ;
#23628 = CARTESIAN_POINT ( 'NONE',  ( 0.000000000000000000, 0.4232283464566928832, -3.341531889763779686E-17 ) ) ;
#23629 = CARTESIAN_POINT ( 'NONE',  ( 0.6342142812959871145, 0.1111449751014438880, 0.2359405056220046093 ) ) ;
#23630 = VECTOR ( 'NONE', #21025, 39.37007874015748143 ) ;
#23631 = DIRECTION ( 'NONE',  ( 1.000000000000000000, 0.000000000000000000, 0.000000000000000000 ) ) ;
#23632 = CIRCLE ( 'NONE', #10068, 0.3149606299212598381 ) ;
#23633 = CARTESIAN_POINT ( 'NONE',  ( 0.4954197419818043846, -0.2442565704126259674, 0.9399606299212598381 ) ) ;
#23634 = LINE ( 'NONE', #334, #10113 ) ;
#23635 = ORIENTED_EDGE ( 'NONE', *, *, #8552, .F. ) ;
#23636 = CARTESIAN_POINT ( 'NONE',  ( -0.7874015748031496509, -3.035194737716535704E-06, -1.475314960619023674 ) ) ;
#23637 = CIRCLE ( 'NONE', #25884, 0.07677362204724409722 ) ;
#23638 = AXIS2_PLACEMENT_3D ( 'NONE', #2512, #9846, #18445 ) ;
#23639 = B_SPLINE_CURVE_WITH_KNOTS ( 'NONE', 3,
 ( #22756, #16837, #16535, #6110, #25445, #7936, #16693, #5678 ),
 .UNSPECIFIED., .F., .F.,
 ( 4, 2, 2, 4 ),
 ( 0.5000000000000000000, 0.7500000000000003331, 0.8750000000000002220, 1.000000000000000000 ),
 .UNSPECIFIED. ) ;
#23640 = EDGE_LOOP ( 'NONE', ( #16937, #13582, #9416, #972 ) ) ;
#23641 = CIRCLE ( 'NONE', #5576, 0.5531496062992126150 ) ;
#23642 = ORIENTED_EDGE ( 'NONE', *, *, #9683, .T. ) ;
#23643 = CARTESIAN_POINT ( 'NONE',  ( 0.3483115186085852799, -0.4538422614029385405, 0.9399606299212601712 ) ) ;
#23644 = CARTESIAN_POINT ( 'NONE',  ( -0.002724751885584015491, -0.1704774416898501010, 0.09842519685039370636 ) ) ;
#23645 = DIRECTION ( 'NONE',  ( 0.000000000000000000, 0.000000000000000000, -1.000000000000000000 ) ) ;
#23646 = CARTESIAN_POINT ( 'NONE',  ( -0.5314946440730490274, -0.03488411621207028468, 1.747047244094488416 ) ) ;
#23647 = ADVANCED_FACE ( 'NONE', ( #1270 ), #25886, .T. ) ;
#23648 = CLOSED_SHELL ( 'NONE', ( #23870, #1032, #26955, #1769, #6207, #9452, #20528, #16242 ) ) ;
#23649 = DIRECTION ( 'NONE',  ( 0.000000000000000000, -1.000000000000000000, 0.000000000000000000 ) ) ;
#23650 = ORIENTED_EDGE ( 'NONE', *, *, #8676, .T. ) ;
#23651 = ADVANCED_FACE ( 'NONE', ( #24987 ), #16854, .T. ) ;
#23652 = FACE_OUTER_BOUND ( 'NONE', #795, .T. ) ;
#23653 = CARTESIAN_POINT ( 'NONE',  ( 0.1490609433576163545, 0.2393035190829114200, 0.4144858534816307505 ) ) ;
#23654 = CARTESIAN_POINT ( 'NONE',  ( -0.3988311005573527690, 0.4763376377694653607, 0.2574803149606298969 ) ) ;
#23655 = EDGE_CURVE ( 'NONE', #11206, #20886, #12377, .T. ) ;
#23656 = EDGE_LOOP ( 'NONE', ( #10066, #19486, #22488, #7824 ) ) ;
#23657 = DIRECTION ( 'NONE',  ( 0.000000000000000000, -1.000000000000000000, 0.000000000000000000 ) ) ;
#23658 = VECTOR ( 'NONE', #22213, 39.37007874015748143 ) ;
#23659 = FACE_OUTER_BOUND ( 'NONE', #16045, .T. ) ;
#23660 = EDGE_CURVE ( 'NONE', #13737, #14598, #14717, .T. ) ;
#23661 = EDGE_CURVE ( 'NONE', #14534, #5538, #14273, .T. ) ;
#23662 = VECTOR ( 'NONE', #11050, 39.37007874015748143 ) ;
#23663 = VERTEX_POINT ( 'NONE', #10020 ) ;
#23664 = CARTESIAN_POINT ( 'NONE',  ( 0.2466292688015071233, 0.4270824798167958125, -1.550196850393700920 ) ) ;
#23665 = DIRECTION ( 'NONE',  ( 0.000000000000000000, 0.000000000000000000, 1.000000000000000000 ) ) ;
#23666 = CARTESIAN_POINT ( 'NONE',  ( 0.3929158813954875540, -0.2268989272875726881, -1.934055118110236338 ) ) ;
#23667 = AXIS2_PLACEMENT_3D ( 'NONE', #21364, #75, #2275 ) ;
#23668 = CARTESIAN_POINT ( 'NONE',  ( -0.2315507648392299000, -0.4792806379917101678, 0.3401574803149606252 ) ) ;
#23669 = CARTESIAN_POINT ( 'NONE',  ( -0.5546128944410685380, -0.3606719828935669447, 0.1849095013362464512 ) ) ;
#23670 = CARTESIAN_POINT ( 'NONE',  ( -0.7874015748031496509, 5.862181872598426086E-06, -1.869015748010449007 ) ) ;
#23671 = ORIENTED_EDGE ( 'NONE', *, *, #16737, .F. ) ;
#23672 = ORIENTED_EDGE ( 'NONE', *, *, #1409, .T. ) ;
#23673 = TOROIDAL_SURFACE ( 'NONE', #4686, 0.5393700787401575214, 0.01181102362204724393 ) ;
#23674 = DIRECTION ( 'NONE',  ( -1.000000000000000000, 0.000000000000000000, 0.000000000000000000 ) ) ;
#23675 = VECTOR ( 'NONE', #18005, 39.37007874015748854 ) ;
#23676 = FACE_OUTER_BOUND ( 'NONE', #116, .T. ) ;
#23677 = CARTESIAN_POINT ( 'NONE',  ( 0.2256062985789750452, -0.6178563876572671365, 0.2081850588211440756 ) ) ;
#23678 = CARTESIAN_POINT ( 'NONE',  ( -0.7246715730664488042, 0.1903343190505137617, -0.09717118172266910048 ) ) ;
#23679 = ORIENTED_EDGE ( 'NONE', *, *, #18752, .F. ) ;
#23680 = ADVANCED_FACE ( 'NONE', ( #8333 ), #16512, .F. ) ;
#23681 = CARTESIAN_POINT ( 'NONE',  ( 0.1447526197146039584, -0.3977045540727763839, 0.1377952755905511861 ) ) ;
#23682 = DIRECTION ( 'NONE',  ( 0.000000000000000000, -1.000000000000000000, 0.000000000000000000 ) ) ;
#23683 = CARTESIAN_POINT ( 'NONE',  ( 0.1839420097223035677, -0.5417097841048799101, 0.9399606299212598381 ) ) ;
#23684 = EDGE_CURVE ( 'NONE', #21791, #16455, #10219, .T. ) ;
#23685 = CARTESIAN_POINT ( 'NONE',  ( 0.1120675189988346587, -0.7410715175625038897, 0.001857066358701496122 ) ) ;
#23686 = FACE_OUTER_BOUND ( 'NONE', #2181, .T. ) ;
#23687 = EDGE_CURVE ( 'NONE', #3579, #21409, #12904, .T. ) ;
#23688 = CIRCLE ( 'NONE', #10573, 0.3722026523000413478 ) ;
#23689 = CARTESIAN_POINT ( 'NONE',  ( 0.3726024258163779246, -0.02438677169350792623, -3.115157480314960647 ) ) ;
#23690 = EDGE_CURVE ( 'NONE', #11735, #17779, #19576, .T. ) ;
#23691 = CARTESIAN_POINT ( 'NONE',  ( -0.02576258704323625137, 0.2165354330708661734, -3.644091798884676159 ) ) ;
#23692 = DIRECTION ( 'NONE',  ( -0.000000000000000000, -1.000000000000000000, -0.000000000000000000 ) ) ;
#23693 = DIRECTION ( 'NONE',  ( 0.000000000000000000, -1.000000000000000000, 0.000000000000000000 ) ) ;
#23694 = DIRECTION ( 'NONE',  ( 1.000000000000000000, 0.000000000000000000, 0.000000000000000000 ) ) ;
#23695 = DIRECTION ( 'NONE',  ( 0.000000000000000000, 0.000000000000000000, 1.000000000000000000 ) ) ;
#23696 = CARTESIAN_POINT ( 'NONE',  ( -0.6117448998508603353, 0.1083144418130620040, 0.2574819594177531479 ) ) ;
#23697 = CIRCLE ( 'NONE', #27288, 0.2952755905511805778 ) ;
#23698 = ORIENTED_EDGE ( 'NONE', *, *, #8536, .T. ) ;
#23699 = ORIENTED_EDGE ( 'NONE', *, *, #8559, .F. ) ;
#23700 = ORIENTED_EDGE ( 'NONE', *, *, #6090, .F. ) ;
#23701 = CARTESIAN_POINT ( 'NONE',  ( 0.3529960615039756111, 0.06172929298871281112, 0.09506557083684616383 ) ) ;
#23702 = CARTESIAN_POINT ( 'NONE',  ( 0.4537304931026562849, 0.07942646906837143306, 0.1771653543307087630 ) ) ;
#23703 = CARTESIAN_POINT ( 'NONE',  ( -0.06699507805369578350, -0.5085118447801426633, 1.766732283464566899 ) ) ;
#23704 = AXIS2_PLACEMENT_3D ( 'NONE', #6194, #27802, #15090 ) ;
#23705 = CARTESIAN_POINT ( 'NONE',  ( 0.000000000000000000, 0.000000000000000000, 0.09685039370078740717 ) ) ;
#23706 = ORIENTED_EDGE ( 'NONE', *, *, #2268, .T. ) ;
#23707 = ORIENTED_EDGE ( 'NONE', *, *, #9655, .T. ) ;
#23709 = CARTESIAN_POINT ( 'NONE',  ( -0.3392387706403586223, -0.1151913129404420061, -3.115157480314960647 ) ) ;
#23708 = CARTESIAN_POINT ( 'NONE',  ( -0.6476458834297724731, 0.1148891961921066213, 0.2081850588258900292 ) ) ;
#23710 = ORIENTED_EDGE ( 'NONE', *, *, #233, .T. ) ;
#23711 = ORIENTED_EDGE ( 'NONE', *, *, #18282, .F. ) ;
#23712 = CARTESIAN_POINT ( 'NONE',  ( -0.2720459371704843088, 0.3242117229735834716, 0.1377952755905511861 ) ) ;
#23713 = CARTESIAN_POINT ( 'NONE',  ( 0.3561571326799479742, 0.7445305536541476643, -0.7131136604161752990 ) ) ;
#23714 = CARTESIAN_POINT ( 'NONE',  ( -0.3007905576423873240, 0.1482986320106437494, 1.973425196850393970 ) ) ;
#23715 = CARTESIAN_POINT ( 'NONE',  ( -0.02576258753924276154, 0.2165354330708661457, -3.644091798679223615 ) ) ;
#23716 = ORIENTED_EDGE ( 'NONE', *, *, #22494, .T. ) ;
#23717 = ORIENTED_EDGE ( 'NONE', *, *, #6964, .F. ) ;
#23719 = EDGE_CURVE ( 'NONE', #3153, #11508, #23028, .T. ) ;
#23718 = VECTOR ( 'NONE', #17269, 39.37007874015748143 ) ;
#23720 = CARTESIAN_POINT ( 'NONE',  ( 0.6117833106355984318, 0.1080972763116263835, 0.09684793308443542803 ) ) ;
#23721 = VECTOR ( 'NONE', #6797, 39.37007874015748143 ) ;
#23722 = ORIENTED_EDGE ( 'NONE', *, *, #13451, .F. ) ;
#23723 = ORIENTED_EDGE ( 'NONE', *, *, #27274, .T. ) ;
#23724 = EDGE_LOOP ( 'NONE', ( #19857, #5055, #25687, #6322 ) ) ;
#23725 = CARTESIAN_POINT ( 'NONE',  ( 0.1109424284362303254, 0.000000000000000000, 0.000000000000000000 ) ) ;
#23726 = EDGE_CURVE ( 'NONE', #26700, #27631, #19195, .T. ) ;
#23727 = DIRECTION ( 'NONE',  ( 1.000000000000000000, 0.000000000000000000, 0.000000000000000000 ) ) ;
#23728 = CYLINDRICAL_SURFACE ( 'NONE', #6528, 0.3149606299212598381 ) ;
#23729 = EDGE_LOOP ( 'NONE', ( #4384, #10866 ) ) ;
#23730 = EDGE_CURVE ( 'NONE', #22824, #11643, #11430, .T. ) ;
#23731 = CARTESIAN_POINT ( 'NONE',  ( -0.5189874374926378708, -0.1182276436463389618, 0.3401599409343964431 ) ) ;
#23732 = CARTESIAN_POINT ( 'NONE',  ( -0.4031801809406276860, -0.9361362132892122601, -0.1635458728543118245 ) ) ;
#23733 = DIRECTION ( 'NONE',  ( -0.9009688679024190350, 0.4338837391175582314, 0.000000000000000000 ) ) ;
#23734 = CIRCLE ( 'NONE', #24603, 0.2952755905264887182 ) ;
#23735 = LINE ( 'NONE', #21472, #25008 ) ;
#23736 = CARTESIAN_POINT ( 'NONE',  ( 0.0006568023596644008595, 0.5148705051078593664, 0.1473214333209106885 ) ) ;
#23737 = AXIS2_PLACEMENT_3D ( 'NONE', #11353, #26452, #22222 ) ;
#23738 = CARTESIAN_POINT ( 'NONE',  ( -0.09842519685039377575, 0.2165354330708661457, -3.259751644589249597 ) ) ;
#23739 = ORIENTED_EDGE ( 'NONE', *, *, #86, .T. ) ;
#23740 = ORIENTED_EDGE ( 'NONE', *, *, #24541, .T. ) ;
#23741 = CARTESIAN_POINT ( 'NONE',  ( 0.000000000000000000, 0.000000000000000000, -0.1756889763779527769 ) ) ;
#23742 = SHAPE_REPRESENTATION_RELATIONSHIP ( 'NONE' , 'NONE' ,  #713, #15726 ) ;
#23743 = ORIENTED_EDGE ( 'NONE', *, *, #7398, .T. ) ;
#23744 = EDGE_CURVE ( 'NONE', #1806, #24677, #21875, .T. ) ;
#23745 = VERTEX_POINT ( 'NONE', #23462 ) ;
#23746 = FACE_OUTER_BOUND ( 'NONE', #9425, .T. ) ;
#23747 = CARTESIAN_POINT ( 'NONE',  ( -0.5610236220428271858, 1.122047244090071949, 1.311930826979132746E-15 ) ) ;
#23748 = DIRECTION ( 'NONE',  ( -0.000000000000000000, -1.000000000000000000, -0.000000000000000000 ) ) ;
#23749 = VERTEX_POINT ( 'NONE', #4091 ) ;
#23750 = CARTESIAN_POINT ( 'NONE',  ( 0.3642352168757554964, -0.4152525734086275899, 0.9202755905511811330 ) ) ;
#23751 = ADVANCED_FACE ( 'NONE', ( #6632 ), #4627, .T. ) ;
#23752 = CARTESIAN_POINT ( 'NONE',  ( 0.3924375359097452831, 0.3121297331107421580, 0.3080453759670797043 ) ) ;
#23753 = ORIENTED_EDGE ( 'NONE', *, *, #9476, .F. ) ;
#23754 = AXIS2_PLACEMENT_3D ( 'NONE', #13426, #26555, #11315 ) ;
#23755 = CARTESIAN_POINT ( 'NONE',  ( 0.000000000000000000, 0.000000000000000000, -3.278217716535432842E-17 ) ) ;
#23756 = DIRECTION ( 'NONE',  ( 1.000000000000000000, 0.000000000000000000, 0.000000000000000000 ) ) ;
#23757 = FACE_OUTER_BOUND ( 'NONE', #3779, .T. ) ;
#23758 = VECTOR ( 'NONE', #17272, 39.37007874015748854 ) ;
#23759 = DIRECTION ( 'NONE',  ( 1.000000000000000000, 0.000000000000000000, 0.000000000000000000 ) ) ;
#23760 = DIRECTION ( 'NONE',  ( 1.000000000000000000, 0.000000000000000000, 0.000000000000000000 ) ) ;
#23761 = FACE_OUTER_BOUND ( 'NONE', #6472, .T. ) ;
#23762 = DIRECTION ( 'NONE',  ( 0.000000000000000000, 0.000000000000000000, -1.000000000000000000 ) ) ;
#23763 = CARTESIAN_POINT ( 'NONE',  ( -2.685748425196850164E-17, 0.000000000000000000, -3.115157480314960647 ) ) ;
#23764 = EDGE_CURVE ( 'NONE', #2394, #19464, #9508, .T. ) ;
#23765 = CARTESIAN_POINT ( 'NONE',  ( 0.000000000000000000, 0.000000000000000000, 0.2362204724409449064 ) ) ;
#23766 = CARTESIAN_POINT ( 'NONE',  ( 0.2647715730835492609, -0.5498038367121063086, 0.2362204724409449064 ) ) ;
#23767 = CARTESIAN_POINT ( 'NONE',  ( -0.03736310157557653361, -0.5708661417322835607, 0.9399606299212598381 ) ) ;
#23768 = DIRECTION ( 'NONE',  ( 0.000000000000000000, 1.000000000000000000, 0.000000000000000000 ) ) ;
#23769 = CARTESIAN_POINT ( 'NONE',  ( -2.685748425196850164E-17, 0.000000000000000000, -3.115157480314960647 ) ) ;
#23770 = EDGE_LOOP ( 'NONE', ( #15900, #311 ) ) ;
#23771 = DIRECTION ( 'NONE',  ( -1.000000000000000000, 0.000000000000000000, 0.000000000000000000 ) ) ;
#23772 = ADVANCED_FACE ( 'NONE', ( #9005 ), #23192, .T. ) ;
#23773 = PRODUCT_DEFINITION_FORMATION_WITH_SPECIFIED_SOURCE ( 'ANY', '', #3449, .NOT_KNOWN. ) ;
#23774 = ORIENTED_EDGE ( 'NONE', *, *, #20642, .F. ) ;
#23775 = AXIS2_PLACEMENT_3D ( 'NONE', #14328, #25862, #3713 ) ;
#23776 = ORIENTED_EDGE ( 'NONE', *, *, #16746, .T. ) ;
#23777 = ORIENTED_EDGE ( 'NONE', *, *, #17135, .F. ) ;
#23778 = CARTESIAN_POINT ( 'NONE',  ( -0.4921259842519685179, 0.000000000000000000, -1.550196850393700920 ) ) ;
#23779 = ADVANCED_FACE ( 'NONE', ( #17626 ), #10527, .F. ) ;
#23780 = CARTESIAN_POINT ( 'NONE',  ( -0.3986320731132245165, -0.2308081338369633029, 0.1639447408623057878 ) ) ;
#23781 = CARTESIAN_POINT ( 'NONE',  ( 0.1257482708760437329, -0.3439950301959718848, 0.1910323753063126184 ) ) ;
#23782 = CARTESIAN_POINT ( 'NONE',  ( 0.5187889641967551313, -0.1190953285357214675, 0.1322834645669291320 ) ) ;
#23783 = VERTEX_POINT ( 'NONE', #17083 ) ;
#23784 = EDGE_CURVE ( 'NONE', #11118, #12651, #12973, .T. ) ;
#23785 = CARTESIAN_POINT ( 'NONE',  ( 0.6397637795275591399, 0.000000000000000000, 0.000000000000000000 ) ) ;
#23786 = DIRECTION ( 'NONE',  ( -1.000000000000000000, 0.000000000000000000, 0.000000000000000000 ) ) ;
#23787 = CARTESIAN_POINT ( 'NONE',  ( 0.4068047116061080937, 0.4858504993705154984, 0.2481708550949471570 ) ) ;
#23788 = B_SPLINE_CURVE_WITH_KNOTS ( 'NONE', 3,
 ( #14573, #1684, #17362, #11135, #10726, #10859 ),
 .UNSPECIFIED., .F., .F.,
 ( 4, 2, 4 ),
 ( 4.333759502428735381E-14, 0.0007294371397779527647, 0.001458874279512567800 ),
 .UNSPECIFIED. ) ;
#23789 = LINE ( 'NONE', #25902, #26301 ) ;
#23790 = AXIS2_PLACEMENT_3D ( 'NONE', #16927, #1799, #24712 ) ;
#23791 = VERTEX_POINT ( 'NONE', #19472 ) ;
#23792 = LINE ( 'NONE', #2438, #6684 ) ;
#23793 = CARTESIAN_POINT ( 'NONE',  ( 0.000000000000000000, 0.000000000000000000, 0.2574803149606298969 ) ) ;
#23794 = DIRECTION ( 'NONE',  ( 0.000000000000000000, -1.000000000000000000, 0.000000000000000000 ) ) ;
#23795 = CARTESIAN_POINT ( 'NONE',  ( -0.4669911931914605407, 0.1585706980422390278, -1.550196850393700920 ) ) ;
#23796 = PRODUCT_DEFINITION_CONTEXT ( 'detailed design', #24776, 'design' ) ;
#23797 = CARTESIAN_POINT ( 'NONE',  ( 0.4382752542996382616, -0.1173917140416361471, -1.934055118110236338 ) ) ;
#23798 = EDGE_CURVE ( 'NONE', #7673, #5072, #4505, .T. ) ;
#23799 = CARTESIAN_POINT ( 'NONE',  ( 0.07874015748031495954, -0.04546065111729338803, -0.3779527559055118058 ) ) ;
#23800 = CARTESIAN_POINT ( 'NONE',  ( -0.3661417322834645272, -0.4724409448818898127, 0.8182917201112815953 ) ) ;
#23801 = B_SPLINE_CURVE_WITH_KNOTS ( 'NONE', 3,
 ( #22503, #22926, #754, #22360, #17950, #11905, #26585, #2984, #24893, #5113 ),
 .UNSPECIFIED., .F., .F.,
 ( 4, 2, 2, 2, 4 ),
 ( 0.000000000000000000, 0.2500000000000000000, 0.5000000000000000000, 0.7500000000000000000, 1.000000000000000000 ),
 .UNSPECIFIED. ) ;
#23802 = FILL_AREA_STYLE ('',( #19274 ) ) ;
#23803 = EDGE_LOOP ( 'NONE', ( #4282, #16678, #18782, #19992, #13296, #19117 ) ) ;
#23804 = CARTESIAN_POINT ( 'NONE',  ( -0.6709908451338839619, -0.1528902114222549236, 0.3401599409343967761 ) ) ;
#23805 = ADVANCED_FACE ( 'NONE', ( #25978, #15257 ), #23869, .T. ) ;
#23806 = CARTESIAN_POINT ( 'NONE',  ( -0.3543292900373042897, -0.02325127328527671483, 1.953740157480314599 ) ) ;
#23807 = VECTOR ( 'NONE', #23692, 39.37007874015748143 ) ;
#23808 = CARTESIAN_POINT ( 'NONE',  ( -0.3020979083623086536, 0.3591256245825952265, 0.1992125984251968684 ) ) ;
#23809 = ORIENTED_EDGE ( 'NONE', *, *, #14629, .F. ) ;
#23810 = CARTESIAN_POINT ( 'NONE',  ( -0.6996199877990079141, 0.1008405537593297374, -0.2423665665178251771 ) ) ;
#23811 = ORIENTED_EDGE ( 'NONE', *, *, #5730, .F. ) ;
#23812 = CARTESIAN_POINT ( 'NONE',  ( -0.2268989272875546748, 0.3929158813954828355, -1.934055118110236338 ) ) ;
#23813 = CIRCLE ( 'NONE', #11610, 0.7552056691767480290 ) ;
#23814 = FACE_OUTER_BOUND ( 'NONE', #27382, .T. ) ;
#23815 = CARTESIAN_POINT ( 'NONE',  ( 0.5869493968219645641, 0.000000000000000000, 0.000000000000000000 ) ) ;
#23816 = ORIENTED_EDGE ( 'NONE', *, *, #16418, .F. ) ;
#23817 = CARTESIAN_POINT ( 'NONE',  ( -0.3338887748335570560, -1.269220122646561144, -0.8285976369166339062 ) ) ;
#23818 = B_SPLINE_CURVE_WITH_KNOTS ( 'NONE', 3,
 ( #11158, #27608, #10354, #17649, #13280, #10491, #26036, #8393, #15425, #17141 ),
 .UNSPECIFIED., .F., .F.,
 ( 4, 2, 2, 2, 4 ),
 ( 0.000000000000000000, 0.2500000000000001665, 0.5000000000000003331, 0.7500000000000001110, 1.000000000000000000 ),
 .UNSPECIFIED. ) ;
#23819 = CARTESIAN_POINT ( 'NONE',  ( 0.7874015748031496509, 0.000000000000000000, -1.052618110236220428 ) ) ;
#23820 = CARTESIAN_POINT ( 'NONE',  ( 0.04877294052296175797, -0.3702005978258584573, -3.115157480314960647 ) ) ;
#23821 = DIRECTION ( 'NONE',  ( 0.000000000000000000, -1.000000000000000000, 0.000000000000000000 ) ) ;
#23822 = ( NAMED_UNIT ( * ) PLANE_ANGLE_UNIT ( ) SI_UNIT ( $, .RADIAN. ) ) ;
#23823 = DIRECTION ( 'NONE',  ( 0.000000000000000000, 1.000000000000000000, 0.000000000000000000 ) ) ;
#23824 = EDGE_LOOP ( 'NONE', ( #48, #26959, #18748, #23860 ) ) ;
#23825 = CARTESIAN_POINT ( 'NONE',  ( -0.2066929133858267931, -0.6299212598425196763, 7.714310545810098438E-17 ) ) ;
#23826 = ADVANCED_FACE ( 'NONE', ( #2769 ), #22422, .F. ) ;
#23827 = AXIS2_PLACEMENT_3D ( 'NONE', #2170, #4437, #10784 ) ;
#23828 = ORIENTED_EDGE ( 'NONE', *, *, #24514, .F. ) ;
#23829 = DIRECTION ( 'NONE',  ( -0.6427876096865390299, 0.7660444431189783465, 0.000000000000000000 ) ) ;
#23830 = ADVANCED_FACE ( 'NONE', ( #15528, #11679 ), #20301, .F. ) ;
#23831 = B_SPLINE_CURVE_WITH_KNOTS ( 'NONE', 3,
 ( #25050, #12755, #27316, #18968, #1457, #7826 ),
 .UNSPECIFIED., .F., .F.,
 ( 4, 2, 4 ),
 ( 0.5000000000000000000, 0.7500000000000000000, 1.000000000000000000 ),
 .UNSPECIFIED. ) ;
#23832 = ORIENTED_EDGE ( 'NONE', *, *, #6126, .F. ) ;
#23833 = EDGE_CURVE ( 'NONE', #23791, #10626, #26503, .T. ) ;
#23834 = CYLINDRICAL_SURFACE ( 'NONE', #21884, 0.4986013261500205074 ) ;
#23835 = ORIENTED_EDGE ( 'NONE', *, *, #13862, .T. ) ;
#23836 = CARTESIAN_POINT ( 'NONE',  ( 1.446433227339387294E-17, 0.07874015748031491790, -1.574803149606299524 ) ) ;
#23837 = CARTESIAN_POINT ( 'NONE',  ( 0.4537304931026565069, 0.07942646906837144694, 0.1639447408552120455 ) ) ;
#23838 = CARTESIAN_POINT ( 'NONE',  ( -0.4441657790107740866, 0.2564944395515753039, 1.766732283464566899 ) ) ;
#23839 = EDGE_CURVE ( 'NONE', #2567, #16194, #1066, .T. ) ;
#23840 = FACE_OUTER_BOUND ( 'NONE', #1214, .T. ) ;
#23841 = VERTEX_POINT ( 'NONE', #11540 ) ;
#23842 = EDGE_LOOP ( 'NONE', ( #20467, #18255 ) ) ;
#23844 = CARTESIAN_POINT ( 'NONE',  ( -0.2807137536170428715, 0.2462256503456040635, -3.115157480314960647 ) ) ;
#23843 = CARTESIAN_POINT ( 'NONE',  ( 0.5791695622054565673, 0.4608640948051578867, 0.2562996996039434427 ) ) ;
#23845 = ORIENTED_EDGE ( 'NONE', *, *, #10581, .T. ) ;
#23846 = EDGE_CURVE ( 'NONE', #17014, #20821, #21370, .T. ) ;
#23847 = ORIENTED_EDGE ( 'NONE', *, *, #27294, .F. ) ;
#23848 = CARTESIAN_POINT ( 'NONE',  ( 0.3665264996331779601, -0.2116141732283464416, 0.1377952755905511861 ) ) ;
#23849 = DIRECTION ( 'NONE',  ( 0.000000000000000000, 0.000000000000000000, 1.000000000000000000 ) ) ;
#23850 = ADVANCED_BREP_SHAPE_REPRESENTATION ( 'M6 Thin Hex Nut', ( #3447, #11588 ), #15695 ) ;
#23851 = AXIS2_PLACEMENT_3D ( 'NONE', #17650, #2536, #2671 ) ;
#23852 = CARTESIAN_POINT ( 'NONE',  ( -0.2521176338356424518, 0.2211428102655600414, 1.953740157480315043 ) ) ;
#23853 = VERTEX_POINT ( 'NONE', #20155 ) ;
#23854 = ORIENTED_EDGE ( 'NONE', *, *, #25622, .T. ) ;
#23855 = ORIENTED_EDGE ( 'NONE', *, *, #11576, .F. ) ;
#23856 = AXIS2_PLACEMENT_3D ( 'NONE', #22770, #3842, #3395 ) ;
#23857 = CARTESIAN_POINT ( 'NONE',  ( 2.632951206231566310, 0.9448818897637796255, -9.561468503937007847E-18 ) ) ;
#23858 = CIRCLE ( 'NONE', #3512, 0.8267716535433071723 ) ;
#23859 = ORIENTED_EDGE ( 'NONE', *, *, #22554, .F. ) ;
#23860 = ORIENTED_EDGE ( 'NONE', *, *, #18502, .F. ) ;
#23861 = ORIENTED_EDGE ( 'NONE', *, *, #2372, .T. ) ;
#23862 = CYLINDRICAL_SURFACE ( 'NONE', #11743, 1.131889763779527547 ) ;
#23863 = B_SPLINE_CURVE_WITH_KNOTS ( 'NONE', 3,
 ( #13356, #21571, #6738, #21980, #2207, #8708, #6870, #8972, #13087, #15500, #21711, #15632, #11235, #26348, #4874, #2614, #19860, #24235 ),
 .UNSPECIFIED., .F., .F.,
 ( 4, 2, 2, 2, 2, 2, 2, 2, 4 ),
 ( 0.000000000000000000, 0.06250000000000000000, 0.1250000000000000000, 0.1875000000000000000, 0.2500000000000000000, 0.3125000000000000000, 0.3750000000000000000, 0.4375000000000000000, 0.5000000000000000000 ),
 .UNSPECIFIED. ) ;
#23864 = FACE_OUTER_BOUND ( 'NONE', #10764, .T. ) ;
#23865 = CARTESIAN_POINT ( 'NONE',  ( -1.452994488188976472E-16, 0.3149606299212598381, -3.646653543307086576 ) ) ;
#23866 = VECTOR ( 'NONE', #20778, 39.37007874015748143 ) ;
#23867 = CARTESIAN_POINT ( 'NONE',  ( 0.7673390720865624903, 0.5739376981955128798, 0.1014356048888053474 ) ) ;
#23868 = ORIENTED_EDGE ( 'NONE', *, *, #6090, .T. ) ;
#23869 = PLANE ( 'NONE',  #26754 ) ;
#23870 = ADVANCED_FACE ( 'NONE', ( #16068 ), #19098, .T. ) ;
#23871 = AXIS2_PLACEMENT_3D ( 'NONE', #26543, #20484, #20347 ) ;
#23872 = DIRECTION ( 'NONE',  ( 0.000000000000000000, 0.000000000000000000, 1.000000000000000000 ) ) ;
#23873 = CIRCLE ( 'NONE', #855, 0.3593781546537452298 ) ;
#23874 = CARTESIAN_POINT ( 'NONE',  ( -0.5190368482393039606, -0.1180105360553399679, 0.1322818204150990051 ) ) ;
#23875 = DIRECTION ( 'NONE',  ( 0.000000000000000000, 0.000000000000000000, 1.000000000000000000 ) ) ;
#23876 = EDGE_CURVE ( 'NONE', #1165, #13130, #1964, .T. ) ;
#23877 = CARTESIAN_POINT ( 'NONE',  ( 0.04956879678462317029, 0.2165354330708661457, -3.186635197791187757 ) ) ;
#23878 = ORIENTED_EDGE ( 'NONE', *, *, #23302, .T. ) ;
#23879 = CIRCLE ( 'NONE', #1741, 0.1003956692913385990 ) ;
#23880 = CARTESIAN_POINT ( 'NONE',  ( -0.2973550541826790461, 0.3552623538052492869, 0.2048502514528301177 ) ) ;
#23881 = VERTEX_POINT ( 'NONE', #13803 ) ;
#23882 = DIRECTION ( 'NONE',  ( 0.000000000000000000, 1.000000000000000000, 0.000000000000000000 ) ) ;
#23883 = ORIENTED_EDGE ( 'NONE', *, *, #16148, .T. ) ;
#23884 = PLANE ( 'NONE',  #13386 ) ;
#23885 = LINE ( 'NONE', #18930, #1635 ) ;
#23886 = CARTESIAN_POINT ( 'NONE',  ( 0.0007595033562148819414, 0.6881885572739390167, 0.3401574803149606252 ) ) ;
#23887 = ORIENTED_EDGE ( 'NONE', *, *, #23744, .T. ) ;
#23888 = CARTESIAN_POINT ( 'NONE',  ( -0.03607471876262473287, 0.5511811023622048555, 0.9399606299212598381 ) ) ;
#23889 = ORIENTED_EDGE ( 'NONE', *, *, #20618, .F. ) ;
#23890 = CARTESIAN_POINT ( 'NONE',  ( 0.3411065095061437402, 0.06065137456822567580, 0.1478915661283759231 ) ) ;
#23891 = VERTEX_POINT ( 'NONE', #7301 ) ;
#23892 = AXIS2_PLACEMENT_3D ( 'NONE', #25794, #12656, #23821 ) ;
#23893 = EDGE_CURVE ( 'NONE', #2008, #833, #16398, .T. ) ;
#23894 = SURFACE_STYLE_USAGE ( .BOTH. , #6933 ) ;
#23895 = CIRCLE ( 'NONE', #2217, 0.5322834645669292097 ) ;
#23896 = DIRECTION ( 'NONE',  ( 0.000000000000000000, 0.000000000000000000, -1.000000000000000000 ) ) ;
#23897 = CARTESIAN_POINT ( 'NONE',  ( 0.3183792087430821205, -0.6629319518596328287, 0.1960773254418380074 ) ) ;
#23898 = DIRECTION ( 'NONE',  ( -0.2036417511401758251, 0.4895227362422921447, 0.8478782506317885659 ) ) ;
#23899 = CARTESIAN_POINT ( 'NONE',  ( -0.0005114926878551800428, 0.3662580330867932221, 0.1910323753037873884 ) ) ;
#23900 = CARTESIAN_POINT ( 'NONE',  ( 0.4792984784118546893, 0.08391448672373898188, 0.1827409795125537750 ) ) ;
#23901 = AXIS2_PLACEMENT_3D ( 'NONE', #597, #22198, #4962 ) ;
#23902 = CARTESIAN_POINT ( 'NONE',  ( -0.4066108233583488052, -0.2343118354750405585, 0.1992142434433716580 ) ) ;
#23903 = CARTESIAN_POINT ( 'NONE',  ( 0.7874015748031496509, 0.000000000000000000, -1.052618110236220428 ) ) ;
#23904 = EDGE_LOOP ( 'NONE', ( #20429, #16460, #27694, #1476 ) ) ;
#23905 = CARTESIAN_POINT ( 'NONE',  ( -0.5393700787401575214, 6.677700066216866815E-17, -3.278217716535432842E-17 ) ) ;
#23906 = ADVANCED_FACE ( 'NONE', ( #26792 ), #7439, .T. ) ;
#23907 = CARTESIAN_POINT ( 'NONE',  ( -0.3482225189666507403, -0.4539000224941303063, 0.9399606299212598381 ) ) ;
#23908 = DIRECTION ( 'NONE',  ( 0.000000000000000000, 0.000000000000000000, -1.000000000000000000 ) ) ;
#23909 = ORIENTED_EDGE ( 'NONE', *, *, #373, .F. ) ;
#23910 = FACE_BOUND ( 'NONE', #4207, .T. ) ;
#23911 = EDGE_CURVE ( 'NONE', #13649, #6594, #20022, .T. ) ;
#23912 = AXIS2_PLACEMENT_3D ( 'NONE', #18171, #24683, #18460 ) ;
#23913 = VERTEX_POINT ( 'NONE', #24393 ) ;
#23914 = AXIS2_PLACEMENT_3D ( 'NONE', #7182, #22024, #13670 ) ;
#23915 = ORIENTED_EDGE ( 'NONE', *, *, #5854, .F. ) ;
#23916 = ADVANCED_FACE ( 'NONE', ( #9135 ), #17754, .T. ) ;
#23917 = CARTESIAN_POINT ( 'NONE',  ( 0.000000000000000000, 0.000000000000000000, 0.9055118110027171596 ) ) ;
#23918 = CARTESIAN_POINT ( 'NONE',  ( 0.1189624676717044027, -0.3253923344978161825, 0.1478915661284414818 ) ) ;
#23919 = ORIENTED_EDGE ( 'NONE', *, *, #12310, .F. ) ;
#23920 = VERTEX_POINT ( 'NONE', #13515 ) ;
#23921 = EDGE_CURVE ( 'NONE', #10030, #19599, #14617, .T. ) ;
#23922 = ( LENGTH_UNIT ( ) NAMED_UNIT ( * ) SI_UNIT ( $, .METRE. ) ) ;
#23923 = CARTESIAN_POINT ( 'NONE',  ( 0.7171569026277438974, -0.1628805401848839596, 0.1960773254442478020 ) ) ;
#23924 = CIRCLE ( 'NONE', #18469, 0.3937007874015748254 ) ;
#23925 = FILL_AREA_STYLE ('',( #352 ) ) ;
#23926 = AXIS2_PLACEMENT_3D ( 'NONE', #8595, #17353, #11125 ) ;
#23927 = DIRECTION ( 'NONE',  ( 0.000000000000000000, 0.000000000000000000, 1.000000000000000000 ) ) ;
#23928 = CARTESIAN_POINT ( 'NONE',  ( 0.2992781133269515892, -0.6197069291944330427, 0.3401574803149606252 ) ) ;
#23929 = CARTESIAN_POINT ( 'NONE',  ( 0.04991721480923575621, 0.3112151455537437439, -3.634049048173129126 ) ) ;
#23930 = CARTESIAN_POINT ( 'NONE',  ( 0.3912931228432187658, 0.3001918266902420251, -1.550196850393700920 ) ) ;
#23931 = CARTESIAN_POINT ( 'NONE',  ( 0.2297883689023240139, -0.3979194638820313656, -1.928289503579174280 ) ) ;
#23932 = AXIS2_PLACEMENT_3D ( 'NONE', #10456, #7790, #16401 ) ;
#23933 = DIRECTION ( 'NONE',  ( 0.000000000000000000, 0.000000000000000000, -1.000000000000000000 ) ) ;
#23934 = ADVANCED_FACE ( 'NONE', ( #25095 ), #14241, .T. ) ;
#23935 = EDGE_CURVE ( 'NONE', #16194, #13928, #5902, .T. ) ;
#23936 = CARTESIAN_POINT ( 'NONE',  ( -0.0002525749203917906525, 0.6881889763779527325, 0.3401599409343964431 ) ) ;
#23937 = ( NAMED_UNIT ( * ) PLANE_ANGLE_UNIT ( ) SI_UNIT ( $, .RADIAN. ) ) ;
#23938 = CIRCLE ( 'NONE', #17185, 0.3346456692913385988 ) ;
#23939 = CARTESIAN_POINT ( 'NONE',  ( -0.07874015748031495954, 0.005904027120612978866, -0.4653543306978101257 ) ) ;
#23940 = DIRECTION ( 'NONE',  ( 0.000000000000000000, 0.000000000000000000, 1.000000000000000000 ) ) ;
#23941 = DIRECTION ( 'NONE',  ( 0.000000000000000000, 1.000000000000000000, 0.000000000000000000 ) ) ;
#23942 = B_SPLINE_CURVE_WITH_KNOTS ( 'NONE', 3,
 ( #26008, #23899, #4536, #6380, #9037, #18040 ),
 .UNSPECIFIED., .F., .F.,
 ( 4, 2, 4 ),
 ( 0.000000000000000000, 0.2500000000000000000, 0.5000000000000000000 ),
 .UNSPECIFIED. ) ;
#23943 = ORIENTED_EDGE ( 'NONE', *, *, #1720, .F. ) ;
#23944 = CARTESIAN_POINT ( 'NONE',  ( -0.7795729917428700917, 0.2877957735339043421, -0.2883818734248744242 ) ) ;
#23945 = ORIENTED_EDGE ( 'NONE', *, *, #23993, .F. ) ;
#23946 = CARTESIAN_POINT ( 'NONE',  ( -0.1173917140416340377, 0.4382752542996236622, -1.934055118110236338 ) ) ;
#23947 = VECTOR ( 'NONE', #27075, 39.37007874015748143 ) ;
#23948 = DIRECTION ( 'NONE',  ( 0.000000000000000000, 0.000000000000000000, 1.000000000000000000 ) ) ;
#23949 = CARTESIAN_POINT ( 'NONE',  ( -0.3992017438595020229, -0.2298214351608249550, 0.1639447408619164881 ) ) ;
#23950 = CARTESIAN_POINT ( 'NONE',  ( 0.1532705055535415473, -0.8125630895486949390, -0.04838628589907047889 ) ) ;
#23951 = DIRECTION ( 'NONE',  ( 1.000000000000000000, 0.000000000000000000, 0.000000000000000000 ) ) ;
#23952 = EDGE_CURVE ( 'NONE', #17381, #14467, #22727, .T. ) ;
#23953 = CARTESIAN_POINT ( 'NONE',  ( -0.2937477835495413414, -0.3350125228557411239, -1.934055118110236560 ) ) ;
#23954 = CARTESIAN_POINT ( 'NONE',  ( -0.04877294052295848975, -0.3702005978258383068, -3.115157480314960647 ) ) ;
#23955 = CARTESIAN_POINT ( 'NONE',  ( 0.000000000000000000, 0.4724409448818896462, 0.000000000000000000 ) ) ;
#23956 = CARTESIAN_POINT ( 'NONE',  ( 0.0002525749203917322682, 0.6881889763779527325, 0.1322810039474933141 ) ) ;
#23957 = DIRECTION ( 'NONE',  ( -1.000000000000000000, 0.000000000000000000, 0.000000000000000000 ) ) ;
#23958 = ORIENTED_EDGE ( 'NONE', *, *, #14545, .T. ) ;
#23959 = CARTESIAN_POINT ( 'NONE',  ( -0.1152775731717075036, 0.4303822302054133853, -1.934055118110236338 ) ) ;
#23960 = EDGE_CURVE ( 'NONE', #11811, #12052, #23211, .T. ) ;
#23961 = COLOUR_RGB ( '', 0.66274510, 0.83137255, 0.94901961) ;
#23962 = ORIENTED_EDGE ( 'NONE', *, *, #14363, .T. ) ;
#23963 = CARTESIAN_POINT ( 'NONE',  ( -0.4158785340170984557, 0.3322209827720822850, 0.1322818204150988386 ) ) ;
#23964 = CARTESIAN_POINT ( 'NONE',  ( 0.4856708409200646281, 0.1649135259617043880, 1.766732283464566899 ) ) ;
#23965 = DIRECTION ( 'NONE',  ( -0.9790454724845839563, -0.1018208755700888840, 0.1763589297585419768 ) ) ;
#23966 = ORIENTED_EDGE ( 'NONE', *, *, #9320, .T. ) ;
#23967 = VERTEX_POINT ( 'NONE', #14532 ) ;
#23968 = ORIENTED_EDGE ( 'NONE', *, *, #20798, .T. ) ;
#23969 = CARTESIAN_POINT ( 'NONE',  ( -0.3572819248074391996, 0.1213180142433954029, -3.100567304031768057 ) ) ;
#23970 = ORIENTED_EDGE ( 'NONE', *, *, #380, .F. ) ;
#23971 = DIRECTION ( 'NONE',  ( -0.000000000000000000, -0.000000000000000000, -1.000000000000000000 ) ) ;
#23972 = DIRECTION ( 'NONE',  ( 0.000000000000000000, 0.9984511807834832720, 0.05563487747868100380 ) ) ;
#23973 = CARTESIAN_POINT ( 'NONE',  ( -0.1677079028045393438, -0.2904160862623708095, 1.953740157480315043 ) ) ;
#23974 = ORIENTED_EDGE ( 'NONE', *, *, #6150, .T. ) ;
#23975 = ORIENTED_EDGE ( 'NONE', *, *, #1435, .T. ) ;
#23976 = CIRCLE ( 'NONE', #25792, 0.5511811023622047445 ) ;
#23977 = CARTESIAN_POINT ( 'NONE',  ( -2.185478346456693112E-16, 0.000000000000000000, 0.000000000000000000 ) ) ;
#23978 = ORIENTED_EDGE ( 'NONE', *, *, #8643, .T. ) ;
#23979 = ORIENTED_EDGE ( 'NONE', *, *, #17844, .F. ) ;
#23980 = ORIENTED_EDGE ( 'NONE', *, *, #10164, .T. ) ;
#23981 = DIRECTION ( 'NONE',  ( 0.9749279121818237304, 0.2225209339563139488, -0.000000000000000000 ) ) ;
#23983 = EDGE_CURVE ( 'NONE', #8124, #26656, #2753, .T. ) ;
#23984 = AXIS2_PLACEMENT_3D ( 'NONE', #21714, #13220, #10 ) ;
#23985 = B_SPLINE_CURVE_WITH_KNOTS ( 'NONE', 3,
 ( #15005, #6513, #25865, #2397, #11159, #19777 ),
 .UNSPECIFIED., .F., .F.,
 ( 4, 2, 4 ),
 ( 0.000000000000000000, 0.2500000000000000000, 0.5000000000000000000 ),
 .UNSPECIFIED. ) ;
#23986 = CARTESIAN_POINT ( 'NONE',  ( 0.4895462770359960136, 0.6604130065487362478, -0.5726600247964968027 ) ) ;
#23987 = PRODUCT_DEFINITION ( 'UNKNOWN', '', #5786, #6282 ) ;
#23988 = FACE_OUTER_BOUND ( 'NONE', #12017, .T. ) ;
#23989 = CARTESIAN_POINT ( 'NONE',  ( 0.6058062761461652235, 0.9107023032972123566, -0.1406092616970065767 ) ) ;
#23990 = EDGE_CURVE ( 'NONE', #5887, #3730, #4816, .T. ) ;
#23991 = DIRECTION ( 'NONE',  ( -0.2036417511401758251, -0.9790454724845842893, 0.000000000000000000 ) ) ;
#23992 = EDGE_CURVE ( 'NONE', #20032, #20701, #5592, .T. ) ;
#23993 = EDGE_CURVE ( 'NONE', #4856, #2522, #12235, .T. ) ;
#23994 = DIRECTION ( 'NONE',  ( 0.000000000000000000, 1.000000000000000000, 0.000000000000000000 ) ) ;
#23995 = AXIS2_PLACEMENT_3D ( 'NONE', #16271, #12157, #24873 ) ;
#23996 = CARTESIAN_POINT ( 'NONE',  ( 0.4035433070866141780, 0.000000000000000000, 0.000000000000000000 ) ) ;
#23997 = DIRECTION ( 'NONE',  ( 1.224646799147353207E-16, 1.000000000000000000, -0.000000000000000000 ) ) ;
#23998 = CARTESIAN_POINT ( 'NONE',  ( -0.4616918773311228796, 0.000000000000000000, -0.04133858267716535029 ) ) ;
#23999 = LINE ( 'NONE', #21613, #12877 ) ;
#24000 = ORIENTED_EDGE ( 'NONE', *, *, #3115, .F. ) ;
#24001 = CARTESIAN_POINT ( 'NONE',  ( 0.3874223757861530171, 0.3097832252395282260, 0.1734435147339651040 ) ) ;
#24002 = ( LENGTH_UNIT ( ) NAMED_UNIT ( * ) SI_UNIT ( $, .METRE. ) ) ;
#24003 = ORIENTED_EDGE ( 'NONE', *, *, #25984, .F. ) ;
#24004 = CARTESIAN_POINT ( 'NONE',  ( 0.5905511811023621549, 0.000000000000000000, 0.9399606299212598381 ) ) ;
#24005 = DIRECTION ( 'NONE',  ( 0.000000000000000000, 0.000000000000000000, -1.000000000000000000 ) ) ;
#24006 = DIRECTION ( 'NONE',  ( 0.000000000000000000, 0.000000000000000000, -1.000000000000000000 ) ) ;
#24007 = CARTESIAN_POINT ( 'NONE',  ( -0.03937007874015750752, 0.06819097667593998491, -0.3779527559055118058 ) ) ;
#24008 = EDGE_LOOP ( 'NONE', ( #13563, #11087, #14354, #16031 ) ) ;
#24009 = CARTESIAN_POINT ( 'NONE',  ( 0.5476281405333119912, 0.07214854559198101425, 0.9399606299212598381 ) ) ;
#24010 = DIRECTION ( 'NONE',  ( 0.000000000000000000, 0.000000000000000000, 1.000000000000000000 ) ) ;
#24011 = VERTEX_POINT ( 'NONE', #7075 ) ;
#24012 = VECTOR ( 'NONE', #22718, 39.37007874015748143 ) ;
#24013 = EDGE_CURVE ( 'NONE', #13133, #17199, #7176, .T. ) ;
#24014 = CARTESIAN_POINT ( 'NONE',  ( 0.1522836969735573143, 0.4909267390297480382, -0.05591742528025173131 ) ) ;
#24015 = AXIS2_PLACEMENT_3D ( 'NONE', #3645, #1543, #5507 ) ;
#24016 = CARTESIAN_POINT ( 'NONE',  ( 0.2089723435111824623, -0.4324731448915265508, 0.2362204724409445455 ) ) ;
#24017 = CYLINDRICAL_SURFACE ( 'NONE', #3036, 2.066929133858267598 ) ;
#24018 = DIRECTION ( 'NONE',  ( 1.000000000000000000, 0.000000000000000000, 0.000000000000000000 ) ) ;
#24019 = EDGE_CURVE ( 'NONE', #10268, #12707, #1082, .T. ) ;
#24020 = CIRCLE ( 'NONE', #19054, 0.01181102362204724046 ) ;
#24021 = CARTESIAN_POINT ( 'NONE',  ( 0.1707210962531913734, -0.4707890492249701131, 0.09685039370078740717 ) ) ;
#24022 = DIRECTION ( 'NONE',  ( 0.000000000000000000, -1.000000000000000000, 0.000000000000000000 ) ) ;
#24023 = CARTESIAN_POINT ( 'NONE',  ( 0.4792984784026986245, 0.08391448672215147397, 0.09284957165657019285 ) ) ;
#24024 = EDGE_CURVE ( 'NONE', #16539, #26492, #1541, .T. ) ;
#24025 = ORIENTED_EDGE ( 'NONE', *, *, #22350, .T. ) ;
#24026 = CARTESIAN_POINT ( 'NONE',  ( 0.000000000000000000, 0.000000000000000000, 0.1771653543307086520 ) ) ;
#24027 = CARTESIAN_POINT ( 'NONE',  ( -0.3772436174784659646, -0.4300830224589956563, 0.9399606299212598381 ) ) ;
#24028 = PRODUCT_DEFINITION_SHAPE ( 'NONE', 'NONE',  #27903 ) ;
#24029 = LINE ( 'NONE', #9047, #13702 ) ;
#24030 = AXIS2_PLACEMENT_3D ( 'NONE', #11766, #20388, #1046 ) ;
#24031 = EDGE_CURVE ( 'NONE', #1011, #21566, #24333, .T. ) ;
#24032 = AXIS2_PLACEMENT_3D ( 'NONE', #12199, #5862, #22951 ) ;
#24033 = VERTEX_POINT ( 'NONE', #5074 ) ;
#24034 = ORIENTED_EDGE ( 'NONE', *, *, #6709, .F. ) ;
#24035 = AXIS2_PLACEMENT_3D ( 'NONE', #27725, #4127, #21361 ) ;
#24036 = CARTESIAN_POINT ( 'NONE',  ( -0.06699507805605005306, -0.5085118447796763697, -1.550196850393700920 ) ) ;
#24037 = CARTESIAN_POINT ( 'NONE',  ( -0.09842519685039370636, -0.07874015748031495954, 0.04546065111729338803 ) ) ;
#24038 = CARTESIAN_POINT ( 'NONE',  ( 0.000000000000000000, 0.000000000000000000, 0.02362204724409448786 ) ) ;
#24039 = FACE_BOUND ( 'NONE', #14731, .T. ) ;
#24040 = CARTESIAN_POINT ( 'NONE',  ( -0.3759206409296168561, 0.2989751379763687655, 0.2362204724409447676 ) ) ;
#24041 = ORIENTED_EDGE ( 'NONE', *, *, #11071, .T. ) ;
#24042 = CARTESIAN_POINT ( 'NONE',  ( 0.07874015748031495954, 0.04546065111729338803, -0.4724409448818898127 ) ) ;
#24043 = ORIENTED_EDGE ( 'NONE', *, *, #24503, .T. ) ;
#24044 = ADVANCED_FACE ( 'NONE', ( #22599 ), #18483, .F. ) ;
#24045 = CARTESIAN_POINT ( 'NONE',  ( 0.000000000000000000, 0.000000000000000000, -0.3779527559055118058 ) ) ;
#24046 = CARTESIAN_POINT ( 'NONE',  ( 0.7217751814627907381, -0.1639319465206539039, 0.2562996996045692755 ) ) ;
#24047 = CARTESIAN_POINT ( 'NONE',  ( 0.7874015748031325534, 0.3931752036646342097, 0.1748360539849539708 ) ) ;
#24048 = ADVANCED_FACE ( 'NONE', ( #7346, #13846 ), #11860, .T. ) ;
#24049 = AXIS2_PLACEMENT_3D ( 'NONE', #13159, #19938, #11456 ) ;
#24050 = CARTESIAN_POINT ( 'NONE',  ( 0.5981657849660177995, 0.2403521948818897747, 0.4163022132461299263 ) ) ;
#24051 = CARTESIAN_POINT ( 'NONE',  ( 0.1716509673353401599, -0.4704508543867079173, 0.09684874903502814492 ) ) ;
#24052 = AXIS2_PLACEMENT_3D ( 'NONE', #19637, #6916, #308 ) ;
#24053 = VERTEX_POINT ( 'NONE', #1273 ) ;
#24054 = LINE ( 'NONE', #26304, #7136 ) ;
#24055 = CARTESIAN_POINT ( 'NONE',  ( -0.3001918266902340870, -0.3912931228432089403, -1.569881889763779625 ) ) ;
#24056 = EDGE_CURVE ( 'NONE', #10695, #13695, #4671, .T. ) ;
#24057 = CARTESIAN_POINT ( 'NONE',  ( -0.4555658499976152354, -0.06001958459474936169, -1.928289503579151187 ) ) ;
#24058 = ORIENTED_EDGE ( 'NONE', *, *, #21282, .F. ) ;
#24059 = TOROIDAL_SURFACE ( 'NONE', #15927, 0.4232283464566928832, 0.07677165354330708902 ) ;
#24060 = CARTESIAN_POINT ( 'NONE',  ( -0.5476281405333199848, 0.07214854559197045325, 0.9202755905511811330 ) ) ;
#24061 = CIRCLE ( 'NONE', #18638, 0.3722026523000413478 ) ;
#24062 = CARTESIAN_POINT ( 'NONE',  ( -0.5754648248623214224, 0.4579130143384639307, 0.1960773254380976105 ) ) ;
#24063 = CARTESIAN_POINT ( 'NONE',  ( -0.3030032861725269200, 0.3454440660767091886, -1.928289503579165620 ) ) ;
#24064 = CYLINDRICAL_SURFACE ( 'NONE', #23479, 0.7500000000000001110 ) ;
#24065 = ORIENTED_EDGE ( 'NONE', *, *, #5625, .T. ) ;
#24066 = CARTESIAN_POINT ( 'NONE',  ( -0.6434710025615986151, -0.03484970772117712556, -0.07928083200629056082 ) ) ;
#24067 = CYLINDRICAL_SURFACE ( 'NONE', #22645, 0.5511811023622047445 ) ;
#24068 = CYLINDRICAL_SURFACE ( 'NONE', #25148, 0.6614173228346456046 ) ;
#24069 = CIRCLE ( 'NONE', #18647, 0.6881889763779527325 ) ;
#24070 = TOROIDAL_SURFACE ( 'NONE', #2342, 0.1023622047244094474, 0.003937007874015747977 ) ;
#24071 = CARTESIAN_POINT ( 'NONE',  ( 0.3665264996331779601, -0.2116141732283464416, 0.1377952755905511861 ) ) ;
#24072 = CARTESIAN_POINT ( 'NONE',  ( 1.857656692913385893E-16, -0.6193720790381457286, 0.000000000000000000 ) ) ;
#24073 = DIRECTION ( 'NONE',  ( 0.000000000000000000, 0.000000000000000000, 1.000000000000000000 ) ) ;
#24074 = VERTEX_POINT ( 'NONE', #860 ) ;
#24075 = CARTESIAN_POINT ( 'NONE',  ( -0.6806799598997224088, 0.08941145402117105234, 0.2332800728132976564 ) ) ;
#24076 = EDGE_LOOP ( 'NONE', ( #16928, #21974, #5235, #17019 ) ) ;
#24077 = EDGE_LOOP ( 'NONE', ( #10692, #10108 ) ) ;
#24079 = EDGE_CURVE ( 'NONE', #9569, #3368, #1137, .T. ) ;
#24078 = CIRCLE ( 'NONE', #20040, 0.09679133858267717494 ) ;
#24080 = DIRECTION ( 'NONE',  ( -0.000000000000000000, -1.000000000000000000, -0.000000000000000000 ) ) ;
#24081 = DIRECTION ( 'NONE',  ( 0.000000000000000000, -1.000000000000000000, 0.000000000000000000 ) ) ;
#24082 = VECTOR ( 'NONE', #3764, 39.37007874015748143 ) ;
#24083 = CARTESIAN_POINT ( 'NONE',  ( -0.1968503937007874127, -0.07874015748031495954, -0.04546065111729331171 ) ) ;
#24084 = EDGE_CURVE ( 'NONE', #9496, #25577, #18045, .T. ) ;
#24085 = DIRECTION ( 'NONE',  ( 1.000000000000000000, 0.000000000000000000, 0.000000000000000000 ) ) ;
#24086 = CARTESIAN_POINT ( 'NONE',  ( -0.3606853515406215904, -0.09660931395005714628, -3.115157480314960647 ) ) ;
#24087 = DIRECTION ( 'NONE',  ( 0.000000000000000000, 1.000000000000000000, 0.000000000000000000 ) ) ;
#24088 = CARTESIAN_POINT ( 'NONE',  ( 0.000000000000000000, 0.6881889763779527325, 0.1322810039474933141 ) ) ;
#24089 = CARTESIAN_POINT ( 'NONE',  ( 0.000000000000000000, 0.000000000000000000, -0.1309055118110236116 ) ) ;
#24090 = AXIS2_PLACEMENT_3D ( 'NONE', #14609, #1721, #12463 ) ;
#24091 = ORIENTED_EDGE ( 'NONE', *, *, #24698, .F. ) ;
#24092 = DIRECTION ( 'NONE',  ( 1.000000000000000000, -1.147443000000000016E-15, 0.000000000000000000 ) ) ;
#24093 = AXIS2_PLACEMENT_3D ( 'NONE', #26721, #27166, #7668 ) ;
#24094 = VERTEX_POINT ( 'NONE', #22459 ) ;
#24095 = AXIS2_PLACEMENT_3D ( 'NONE', #4003, #10483, #6265 ) ;
#24096 = VERTEX_POINT ( 'NONE', #3088 ) ;
#24097 = CARTESIAN_POINT ( 'NONE',  ( 0.000000000000000000, 0.000000000000000000, 0.02362204724409448786 ) ) ;
#24098 = CARTESIAN_POINT ( 'NONE',  ( 0.000000000000000000, 0.000000000000000000, 0.000000000000000000 ) ) ;
#24099 = SHAPE_DEFINITION_REPRESENTATION ( #22464, #713 ) ;
#24100 = CARTESIAN_POINT ( 'NONE',  ( 0.1649135259616801574, 0.4856708409200201637, 1.747047244094488194 ) ) ;
#24101 = CARTESIAN_POINT ( 'NONE',  ( 0.000000000000000000, 0.000000000000000000, 0.2374015748031496065 ) ) ;
#24102 = ORIENTED_EDGE ( 'NONE', *, *, #13853, .F. ) ;
#24103 = ORIENTED_EDGE ( 'NONE', *, *, #12206, .T. ) ;
#24104 = VERTEX_POINT ( 'NONE', #11719 ) ;
#24106 = CARTESIAN_POINT ( 'NONE',  ( 0.09660931395005890876, 0.3606853515406323596, -3.115157480314960647 ) ) ;
#24105 = DIRECTION ( 'NONE',  ( 0.000000000000000000, 1.000000000000000000, 0.000000000000000000 ) ) ;
#24107 = ORIENTED_EDGE ( 'NONE', *, *, #13842, .F. ) ;
#24108 = CARTESIAN_POINT ( 'NONE',  ( 0.8267716535433071723, 0.000000000000000000, 0.02362204724409448786 ) ) ;
#24109 = VERTEX_POINT ( 'NONE', #24704 ) ;
#24110 = CARTESIAN_POINT ( 'NONE',  ( 0.4684132450478833976, -0.1062614382955264641, 0.2362204724409446843 ) ) ;
#24111 = AXIS2_PLACEMENT_3D ( 'NONE', #2775, #22017, #15930 ) ;
#24112 = CARTESIAN_POINT ( 'NONE',  ( -0.08676778863011463949, -0.3239425792934414461, 1.953740157480315043 ) ) ;
#24113 = ORIENTED_EDGE ( 'NONE', *, *, #15114, .T. ) ;
#24114 = EDGE_LOOP ( 'NONE', ( #14967, #407, #21651, #11522, #12563, #25829 ) ) ;
#24115 = PLANE ( 'NONE',  #19988 ) ;
#24116 = ORIENTED_EDGE ( 'NONE', *, *, #2570, .T. ) ;
#24117 = EDGE_LOOP ( 'NONE', ( #14109, #24648, #13102, #3070 ) ) ;
#24118 = EDGE_LOOP ( 'NONE', ( #12145, #1982, #10562, #22583, #15509, #1059, #2491, #21012 ) ) ;
#24119 = CARTESIAN_POINT ( 'NONE',  ( 0.06881554280502791276, 0.1968503937007874127, -3.587858213119324180 ) ) ;
#24120 = EDGE_CURVE ( 'NONE', #22088, #15780, #7634, .T. ) ;
#24121 = AXIS2_PLACEMENT_3D ( 'NONE', #2114, #19203, #14580 ) ;
#24122 = FACE_OUTER_BOUND ( 'NONE', #3207, .T. ) ;
#24123 = AXIS2_PLACEMENT_3D ( 'NONE', #2063, #1505, #1653 ) ;
#24124 = CARTESIAN_POINT ( 'NONE',  ( -0.3183792087428392037, -0.6629319518591524352, 0.1960773254403069543 ) ) ;
#24125 = CARTESIAN_POINT ( 'NONE',  ( 0.09842519685039370636, 0.2165354330708661457, -3.272637795275590733 ) ) ;
#24126 = DIRECTION ( 'NONE',  ( -0.1772802999855984940, 0.000000000000000000, 0.9841604011730080703 ) ) ;
#24127 = AXIS2_PLACEMENT_3D ( 'NONE', #23291, #23430, #14685 ) ;
#24128 = CARTESIAN_POINT ( 'NONE',  ( 0.3214446924536846772, 0.3840069416942866742, 0.2574803149606298969 ) ) ;
#24129 = CARTESIAN_POINT ( 'NONE',  ( 0.000000000000000000, 0.000000000000000000, 0.000000000000000000 ) ) ;
#24130 = CARTESIAN_POINT ( 'NONE',  ( -0.4333973147258542991, -0.2509079296564011852, 0.2574803149606298969 ) ) ;
#24131 = CARTESIAN_POINT ( 'NONE',  ( -0.3070866141732283561, 3.760726391082423050E-17, 0.2637795275590551491 ) ) ;
#24132 = EDGE_CURVE ( 'NONE', #24341, #8473, #6052, .T. ) ;
#24133 = B_SPLINE_CURVE_WITH_KNOTS ( 'NONE', 3,
 ( #24597, #27160, #16410, #12166, #18073, #1171 ),
 .UNSPECIFIED., .F., .F.,
 ( 4, 2, 4 ),
 ( 0.6902184472752670441, 0.6915327610580710438, 0.6928470748408740443 ),
 .UNSPECIFIED. ) ;
#24134 = CARTESIAN_POINT ( 'NONE',  ( -0.3382184156732166436, 0.3855916753051391033, 1.766732283464566899 ) ) ;
#24135 = ADVANCED_FACE ( 'NONE', ( #5654 ), #18910, .F. ) ;
#24136 = AXIS2_PLACEMENT_3D ( 'NONE', #11175, #26286, #17399 ) ;
#24137 = EDGE_LOOP ( 'NONE', ( #24608, #10142, #13504, #18856, #5837 ) ) ;
#24138 = CARTESIAN_POINT ( 'NONE',  ( 0.000000000000000000, 0.000000000000000000, 0.1992125984251968684 ) ) ;
#24139 = ORIENTED_EDGE ( 'NONE', *, *, #5317, .F. ) ;
#24140 = AXIS2_PLACEMENT_3D ( 'NONE', #3565, #12066, #10078 ) ;
#24141 = LINE ( 'NONE', #17372, #2237 ) ;
#24142 = B_SPLINE_CURVE_WITH_KNOTS ( 'NONE', 3,
 ( #6169, #10801, #2042, #14795, #19418, #23398 ),
 .UNSPECIFIED., .F., .F.,
 ( 4, 2, 4 ),
 ( 0.2376120521391529850, 0.2390783382518560096, 0.2405446243645580073 ),
 .UNSPECIFIED. ) ;
#24143 = ( NAMED_UNIT ( * ) SI_UNIT ( $, .STERADIAN. ) SOLID_ANGLE_UNIT ( ) ) ;
#24144 = ORIENTED_EDGE ( 'NONE', *, *, #6459, .T. ) ;
#24145 = CARTESIAN_POINT ( 'NONE',  ( 0.000000000000000000, 0.000000000000000000, 0.3543307086614173040 ) ) ;
#24146 = ( BOUNDED_CURVE ( )  B_SPLINE_CURVE ( 3, ( #11188, #2560, #468, #15176 ),
 .UNSPECIFIED., .F., .F. ) 
 B_SPLINE_CURVE_WITH_KNOTS ( ( 4, 4 ),
 ( 6.170019055269734487, 6.396351559089437089 ),
 .UNSPECIFIED. ) 
 CURVE ( )  GEOMETRIC_REPRESENTATION_ITEM ( )  RATIONAL_B_SPLINE_CURVE ( ( 1.000000000000000000, 0.9957356870045845909, 0.9957356870045845909, 1.000000000000000000 ) ) 
 REPRESENTATION_ITEM ( '' )  ) ;
#24147 = DIRECTION ( 'NONE',  ( 0.000000000000000000, 0.000000000000000000, -1.000000000000000000 ) ) ;
#24148 = DIRECTION ( 'NONE',  ( 0.000000000000000000, 0.000000000000000000, 1.000000000000000000 ) ) ;
#24149 = ADVANCED_FACE ( 'NONE', ( #5939, #25136 ), #22890, .T. ) ;
#24150 = EDGE_LOOP ( 'NONE', ( #249, #23438, #14698, #8446 ) ) ;
#24151 = CARTESIAN_POINT ( 'NONE',  ( -0.5230301363771269196, -0.1775991818008745282, 0.9202755905511811330 ) ) ;
#24152 = AXIS2_PLACEMENT_3D ( 'NONE', #11757, #20381, #1039 ) ;
#24153 = DIRECTION ( 'NONE',  ( -0.9930684569549264040, -0.05876869872891801738, -0.1017903720931950112 ) ) ;
#24154 = VERTEX_POINT ( 'NONE', #10437 ) ;
#24155 = CARTESIAN_POINT ( 'NONE',  ( 1.687505431895960050E-16, 0.1968503937007875237, 1.377952755905512472 ) ) ;
#24156 = CARTESIAN_POINT ( 'NONE',  ( -0.1968503937007874127, -0.07874015748031495954, -0.04546065111729338803 ) ) ;
#24157 = CARTESIAN_POINT ( 'NONE',  ( 8.353478384051541640E-17, 8.115082136941410961E-18, 0.1023622047244094474 ) ) ;
#24158 = CARTESIAN_POINT ( 'NONE',  ( -0.07874015748238459567, 0.03414999754297557560, -0.4724409448841456749 ) ) ;
#24159 = CARTESIAN_POINT ( 'NONE',  ( 0.3346456692913385988, 2.049113738730807321E-17, 1.973425196850393970 ) ) ;
#24160 = DIRECTION ( 'NONE',  ( 0.000000000000000000, 0.000000000000000000, -1.000000000000000000 ) ) ;
#24161 = AXIS2_PLACEMENT_3D ( 'NONE', #6815, #13568, #2687 ) ;
#24162 = CARTESIAN_POINT ( 'NONE',  ( -0.4063220079890716430, -0.2348123150948748239, 0.1992150590373740204 ) ) ;
#24163 = CARTESIAN_POINT ( 'NONE',  ( -0.2362204724409449064, 0.000000000000000000, 0.000000000000000000 ) ) ;
#24164 = CARTESIAN_POINT ( 'NONE',  ( -0.3218517393628410050, 0.3826375019110230258, 0.1496602734613065311 ) ) ;
#24165 = AXIS2_PLACEMENT_3D ( 'NONE', #15901, #5017, #11659 ) ;
#24166 = EDGE_CURVE ( 'NONE', #13350, #12714, #20472, .T. ) ;
#24167 = CARTESIAN_POINT ( 'NONE',  ( -0.5708661417322835607, 0.000000000000000000, 0.9399606299212598381 ) ) ;
#24168 = CARTESIAN_POINT ( 'NONE',  ( 0.3992017438595159562, -0.2298214351608004746, 0.1771653543307084855 ) ) ;
#24169 = CARTESIAN_POINT ( 'NONE',  ( -0.1918813796216842782, -0.5271897577243779276, 0.1771653543307086520 ) ) ;
#24170 = CARTESIAN_POINT ( 'NONE',  ( 0.6299212598425196763, -1.895600393700787470E-35, 0.000000000000000000 ) ) ;
#24171 = CIRCLE ( 'NONE', #21480, 0.07677362204724408334 ) ;
#24172 = CARTESIAN_POINT ( 'NONE',  ( -0.5018154743035343479, -0.1152098006138999320, 0.1473214333322230285 ) ) ;
#24173 = EDGE_CURVE ( 'NONE', #6614, #10848, #16383, .T. ) ;
#24174 = ORIENTED_EDGE ( 'NONE', *, *, #26340, .T. ) ;
#24175 = ADVANCED_FACE ( 'NONE', ( #12138, #18770 ), #20763, .T. ) ;
#24176 = EDGE_CURVE ( 'NONE', #17596, #15474, #19052, .T. ) ;
#24177 = VERTEX_POINT ( 'NONE', #18624 ) ;
#24178 = FACE_OUTER_BOUND ( 'NONE', #19073, .T. ) ;
#24179 = ADVANCED_FACE ( 'NONE', ( #6084, #1548 ), #1402, .T. ) ;
#24180 = VECTOR ( 'NONE', #24277, 39.37007874015748143 ) ;
#24181 = DIRECTION ( 'NONE',  ( 0.000000000000000000, 1.000000000000000000, 0.000000000000000000 ) ) ;
#24182 = CARTESIAN_POINT ( 'NONE',  ( 0.03008364706454716778, 0.2273032555864669124, 0.000000000000000000 ) ) ;
#24183 = ORIENTED_EDGE ( 'NONE', *, *, #15730, .F. ) ;
#24184 = CARTESIAN_POINT ( 'NONE',  ( -0.5905511811023621549, -0.4724409448818898127, 0.6411263657805729155 ) ) ;
#24185 = VERTEX_POINT ( 'NONE', #16515 ) ;
#24186 = AXIS2_PLACEMENT_3D ( 'NONE', #15170, #15316, #4138 ) ;
#24187 = SURFACE_STYLE_FILL_AREA ( #26295 ) ;
#24188 = CARTESIAN_POINT ( 'NONE',  ( -0.6117833106355984318, 0.1080972763116267721, 0.09684793308443542803 ) ) ;
#24189 = CARTESIAN_POINT ( 'NONE',  ( 0.4895462770358314786, 0.6578651782979850760, -0.5745116702929976560 ) ) ;
#24190 = DIRECTION ( 'NONE',  ( -0.3174974722037094410, 0.000000000000000000, -0.9482591181445367834 ) ) ;
#24191 = FACE_BOUND ( 'NONE', #2831, .T. ) ;
#24192 = ORIENTED_EDGE ( 'NONE', *, *, #19595, .F. ) ;
#24193 = CARTESIAN_POINT ( 'NONE',  ( 0.4405067310592692409, 5.394651581945980194E-17, -0.1627508102905848297 ) ) ;
#24194 = B_SPLINE_CURVE_WITH_KNOTS ( 'NONE', 3,
 ( #21846, #17725, #10966, #19994, #2481, #26078, #7274, #15374 ),
 .UNSPECIFIED., .F., .F.,
 ( 4, 2, 2, 4 ),
 ( 0.000000000000000000, 0.1250000000000000000, 0.2500000000000000000, 0.5000000000000000000 ),
 .UNSPECIFIED. ) ;
#24195 = CARTESIAN_POINT ( 'NONE',  ( -0.3001918266902322552, -0.3912931228432061648, -1.550196850393700920 ) ) ;
#24196 = CARTESIAN_POINT ( 'NONE',  ( -0.3454440660767502114, -0.3030032861725112103, -1.928289503579147635 ) ) ;
#24197 = AXIS2_PLACEMENT_3D ( 'NONE', #25566, #23466, #27406 ) ;
#24198 = DIRECTION ( 'NONE',  ( 1.000000000000000000, 0.000000000000000000, 0.000000000000000000 ) ) ;
#24199 = VECTOR ( 'NONE', #15871, 39.37007874015748143 ) ;
#24200 = DIRECTION ( 'NONE',  ( 1.000000000000000000, 0.000000000000000000, 0.000000000000000000 ) ) ;
#24201 = CARTESIAN_POINT ( 'NONE',  ( 0.2307489990847578776, -0.4796672131996535526, 0.3401599409343964431 ) ) ;
#24202 = EDGE_CURVE ( 'NONE', #19937, #22507, #21830, .T. ) ;
#24203 = TOROIDAL_SURFACE ( 'NONE', #19713, 0.4232283464566928832, 0.07677165354330708902 ) ;
#24204 = CARTESIAN_POINT ( 'NONE',  ( -0.6262477747318130339, -0.08149594654892677870, -0.08212545458858977465 ) ) ;
#24205 = CARTESIAN_POINT ( 'NONE',  ( 0.5118110236220472231, 6.267877318470705905E-17, -0.1377952755905511861 ) ) ;
#24206 = EDGE_CURVE ( 'NONE', #830, #7850, #25421, .T. ) ;
#24207 = CARTESIAN_POINT ( 'NONE',  ( 0.3976891862754212137, 1.133679329692560245, -0.4395307839725697274 ) ) ;
#24208 = DIRECTION ( 'NONE',  ( -1.000000000000000000, 0.000000000000000000, 0.000000000000000000 ) ) ;
#24209 = FACE_OUTER_BOUND ( 'NONE', #26857, .T. ) ;
#24210 = DIRECTION ( 'NONE',  ( 0.000000000000000000, 0.000000000000000000, 1.000000000000000000 ) ) ;
#24211 = DIRECTION ( 'NONE',  ( 0.000000000000000000, 0.000000000000000000, 1.000000000000000000 ) ) ;
#24212 = DIRECTION ( 'NONE',  ( 1.000000000000000000, 0.000000000000000000, 0.000000000000000000 ) ) ;
#24213 = DIRECTION ( 'NONE',  ( 0.6234898018587335944, 0.7818314824680296926, 0.000000000000000000 ) ) ;
#24214 = CARTESIAN_POINT ( 'NONE',  ( 0.1522836969735573143, 0.1970374587079574968, -0.4531137400369417145 ) ) ;
#24215 = VERTEX_POINT ( 'NONE', #15577 ) ;
#24216 = FACE_OUTER_BOUND ( 'NONE', #4481, .T. ) ;
#24217 = CARTESIAN_POINT ( 'NONE',  ( 0.4232283464566928832, 0.000000000000000000, 0.1377952755905511861 ) ) ;
#24218 = CONICAL_SURFACE ( 'NONE', #7087, 0.4307823082429378392, 0.9572651268756555698 ) ;
#24219 = AXIS2_PLACEMENT_3D ( 'NONE', #3737, #16598, #1483 ) ;
#24220 = DIRECTION ( 'NONE',  ( -1.000000000000000000, 0.000000000000000000, 0.000000000000000000 ) ) ;
#24221 = CARTESIAN_POINT ( 'NONE',  ( 0.3267488823401797360, -0.1886891683788832486, -3.100567304031763172 ) ) ;
#24222 = CARTESIAN_POINT ( 'NONE',  ( -0.4055118110236220486, -0.4724409448818898127, -0.8182917201112815953 ) ) ;
#24223 = CARTESIAN_POINT ( 'NONE',  ( 0.000000000000000000, 0.000000000000000000, 0.07637795275590551769 ) ) ;
#24224 = DIRECTION ( 'NONE',  ( 0.000000000000000000, 0.000000000000000000, -1.000000000000000000 ) ) ;
#24225 = ORIENTED_EDGE ( 'NONE', *, *, #25951, .T. ) ;
#24226 = CARTESIAN_POINT ( 'NONE',  ( -0.3024344094364737612, -0.3935368318888682881, -1.569881889763779403 ) ) ;
#24227 = DIRECTION ( 'NONE',  ( 0.000000000000000000, 0.000000000000000000, 1.000000000000000000 ) ) ;
#24228 = CARTESIAN_POINT ( 'NONE',  ( -0.3030032861724965554, -0.3454440660767394422, -1.928289503579165620 ) ) ;
#24229 = EDGE_CURVE ( 'NONE', #24517, #22371, #15089, .T. ) ;
#24230 = VERTEX_POINT ( 'NONE', #25754 ) ;
#24231 = EDGE_CURVE ( 'NONE', #23749, #12770, #21390, .T. ) ;
#24232 = AXIS2_PLACEMENT_3D ( 'NONE', #9455, #20351, #26989 ) ;
#24233 = CIRCLE ( 'NONE', #17897, 1.288838582677166222 ) ;
#24234 = CARTESIAN_POINT ( 'NONE',  ( -0.5385210225480960844, 0.4284847435812472183, 0.3401574803149606252 ) ) ;
#24235 = CARTESIAN_POINT ( 'NONE',  ( -0.5118110236220472231, 3.201384367575308305E-17, 1.766732283464566899 ) ) ;
#24236 = CARTESIAN_POINT ( 'NONE',  ( -0.4069448477556031341, -0.3121994997598085408, 1.747047244094488194 ) ) ;
#24237 = EDGE_CURVE ( 'NONE', #8838, #27393, #21786, .T. ) ;
#24238 = PRESENTATION_STYLE_ASSIGNMENT (( #25950 ) ) ;
#24239 = ORIENTED_EDGE ( 'NONE', *, *, #16442, .T. ) ;
#24240 = CARTESIAN_POINT ( 'NONE',  ( 0.2272836761397793726, 0.2962590301041582164, -3.115157480314960647 ) ) ;
#24241 = DIRECTION ( 'NONE',  ( 0.000000000000000000, -1.000000000000000000, 0.000000000000000000 ) ) ;
#24242 = DIRECTION ( 'NONE',  ( -1.000000000000000000, 0.000000000000000000, 0.000000000000000000 ) ) ;
#24243 = CARTESIAN_POINT ( 'NONE',  ( -0.3324885138898230341, 0.04380447413659110945, 1.953740157480315043 ) ) ;
#24244 = ORIENTED_EDGE ( 'NONE', *, *, #2466, .F. ) ;
#24245 = ORIENTED_EDGE ( 'NONE', *, *, #20639, .F. ) ;
#24246 = DIRECTION ( 'NONE',  ( 0.000000000000000000, 1.000000000000000000, 0.000000000000000000 ) ) ;
#24247 = ORIENTED_EDGE ( 'NONE', *, *, #1208, .F. ) ;
#24248 = ORIENTED_EDGE ( 'NONE', *, *, #4448, .T. ) ;
#24249 = ORIENTED_EDGE ( 'NONE', *, *, #11319, .T. ) ;
#24250 = CARTESIAN_POINT ( 'NONE',  ( 0.000000000000000000, 0.000000000000000000, 0.1322834645669291320 ) ) ;
#24251 = EDGE_CURVE ( 'NONE', #26228, #11259, #14965, .T. ) ;
#24252 = DIRECTION ( 'NONE',  ( 0.000000000000000000, 0.000000000000000000, 1.000000000000000000 ) ) ;
#24253 = CARTESIAN_POINT ( 'NONE',  ( -0.3204319178468620910, -0.6672004808830966915, 0.2161412452771441228 ) ) ;
#24254 = CIRCLE ( 'NONE', #21098, 0.5118110236220472231 ) ;
#24255 = CARTESIAN_POINT ( 'NONE',  ( 0.6939626785200878611, 0.7744396987992381298, -0.02240038148060783177 ) ) ;
#24256 = ORIENTED_EDGE ( 'NONE', *, *, #10601, .T. ) ;
#24257 = CARTESIAN_POINT ( 'NONE',  ( 0.6397637795275591399, 0.000000000000000000, 0.000000000000000000 ) ) ;
#24258 = CARTESIAN_POINT ( 'NONE',  ( -0.3074993854542726890, 0.1775730735577450703, 1.953740157480315043 ) ) ;
#24259 = CARTESIAN_POINT ( 'NONE',  ( -0.5187889641967551313, -0.1190953285357212593, 0.3401574803149606252 ) ) ;
#24260 = CARTESIAN_POINT ( 'NONE',  ( -0.2315507648392299000, -0.4792806379917101678, 0.1322834645669291320 ) ) ;
#24261 = LINE ( 'NONE', #11137, #2629 ) ;
#24262 = CARTESIAN_POINT ( 'NONE',  ( -0.4121125639576288524, -0.2386018002113109993, 0.2330651857992618037 ) ) ;
#24263 = PLANE ( 'NONE',  #15148 ) ;
#24264 = EDGE_CURVE ( 'NONE', #6360, #20178, #8784, .T. ) ;
#24265 = CIRCLE ( 'NONE', #6244, 0.2952755905511810774 ) ;
#24266 = EDGE_CURVE ( 'NONE', #18491, #22996, #8920, .T. ) ;
#24267 = AXIS2_PLACEMENT_3D ( 'NONE', #3124, #9624, #14022 ) ;
#24268 = CARTESIAN_POINT ( 'NONE',  ( 0.4327133464951135045, -0.2505177833314600200, 0.1496602734566857273 ) ) ;
#24269 = ORIENTED_EDGE ( 'NONE', *, *, #12206, .F. ) ;
#24270 = TOROIDAL_SURFACE ( 'NONE', #27431, 0.5241918773311228241, 0.01377952755905511792 ) ;
#24271 = DIRECTION ( 'NONE',  ( -1.000000000000000000, 0.000000000000000000, 0.000000000000000000 ) ) ;
#24272 = CARTESIAN_POINT ( 'NONE',  ( -0.1771653543307086520, 1.482715313533957208E-17, 0.1673228346456692994 ) ) ;
#24273 = EDGE_LOOP ( 'NONE', ( #2627, #10550, #19624, #17866, #27736, #24256, #25690, #17303, #15646, #16531, #27258 ) ) ;
#24274 = CARTESIAN_POINT ( 'NONE',  ( -0.3765118517642103702, 0.04928528614549729236, -3.100567304031763616 ) ) ;
#24275 = EDGE_LOOP ( 'NONE', ( #3699, #294, #9758, #26819 ) ) ;
#24276 = SPHERICAL_SURFACE ( 'NONE', #4368, 0.1299232283464566984 ) ;
#24277 = DIRECTION ( 'NONE',  ( 0.000000000000000000, 0.000000000000000000, -1.000000000000000000 ) ) ;
#24278 = CIRCLE ( 'NONE', #12103, 0.4986013261500205074 ) ;
#24279 = VERTEX_POINT ( 'NONE', #19673 ) ;
#24280 = CARTESIAN_POINT ( 'NONE',  ( 0.5511811023622048555, -0.03607471876262468430, 0.9399606299212598381 ) ) ;
#24281 = VERTEX_POINT ( 'NONE', #2012 ) ;
#24282 = DIRECTION ( 'NONE',  ( 0.000000000000000000, 0.000000000000000000, 1.000000000000000000 ) ) ;
#24283 = EDGE_LOOP ( 'NONE', ( #13919, #2353, #1704, #1896, #29, #16178 ) ) ;
#24284 = CARTESIAN_POINT ( 'NONE',  ( 0.000000000000000000, 0.000000000000000000, 1.747047244094488194 ) ) ;
#24285 = CARTESIAN_POINT ( 'NONE',  ( 0.3543307086367249448, 0.000000000000000000, -4.330708661417323135 ) ) ;
#24286 = CARTESIAN_POINT ( 'NONE',  ( -0.1580799066051627177, -0.4326553680327468454, 0.1771653543307088186 ) ) ;
#24287 = DIRECTION ( 'NONE',  ( 0.000000000000000000, 1.000000000000000000, 0.000000000000000000 ) ) ;
#24288 = FACE_OUTER_BOUND ( 'NONE', #13532, .T. ) ;
#24289 = ADVANCED_FACE ( 'NONE', ( #15447, #17670, #6405, #10623, #19249, #26161, #8513, #17133, #17547, #24039 ), #4676, .T. ) ;
#24290 = CIRCLE ( 'NONE', #19798, 0.5322834645669292097 ) ;
#24291 = CARTESIAN_POINT ( 'NONE',  ( 0.000000000000000000, 0.000000000000000000, 0.2362204724409449064 ) ) ;
#24292 = VECTOR ( 'NONE', #10920, 39.37007874015748854 ) ;
#24293 = CARTESIAN_POINT ( 'NONE',  ( 0.3543307086614173596, 0.02319089060379041917, 1.953740157480315043 ) ) ;
#24294 = DIRECTION ( 'NONE',  ( 0.000000000000000000, 0.000000000000000000, 1.000000000000000000 ) ) ;
#24295 = CARTESIAN_POINT ( 'NONE',  ( 0.1520645003235147619, 0.4909313315706889669, -0.05587710509139291737 ) ) ;
#24296 = CARTESIAN_POINT ( 'NONE',  ( 0.3772436174784756235, 0.4300830224589536899, 0.9399606299212598381 ) ) ;
#24297 = CARTESIAN_POINT ( 'NONE',  ( 0.4472135058506041538, -0.2577577458591220338, 1.766732283464566455 ) ) ;
#24298 = EDGE_CURVE ( 'NONE', #17515, #17328, #10099, .T. ) ;
#24299 = AXIS2_PLACEMENT_3D ( 'NONE', #21759, #4248, #11018 ) ;
#24300 = DIRECTION ( 'NONE',  ( 0.000000000000000000, 1.000000000000000000, 0.000000000000000000 ) ) ;
#24301 = ORIENTED_EDGE ( 'NONE', *, *, #19828, .F. ) ;
#24302 = LINE ( 'NONE', #17398, #1999 ) ;
#24303 = ORIENTED_EDGE ( 'NONE', *, *, #25563, .T. ) ;
#24304 = VERTEX_POINT ( 'NONE', #7722 ) ;
#24305 = B_SPLINE_CURVE_WITH_KNOTS ( 'NONE', 3,
 ( #17140, #14907, #2292, #10631, #23518, #21660, #4148, #12757, #23787, #4558 ),
 .UNSPECIFIED., .F., .F.,
 ( 4, 2, 2, 2, 4 ),
 ( 0.000000000000000000, 0.2500000000000000000, 0.5000000000000000000, 0.7500000000000000000, 1.000000000000000000 ),
 .UNSPECIFIED. ) ;
#24306 = VECTOR ( 'NONE', #18920, 39.37007874015748854 ) ;
#24307 = CARTESIAN_POINT ( 'NONE',  ( -0.6614173228346456046, 0.000000000000000000, -0.01377952755905511792 ) ) ;
#24308 = DIRECTION ( 'NONE',  ( 0.000000000000000000, 1.000000000000000000, 0.000000000000000000 ) ) ;
#24309 = AXIS2_PLACEMENT_3D ( 'NONE', #12388, #1370, #27368 ) ;
#24310 = VERTEX_POINT ( 'NONE', #17776 ) ;
#24311 = DIRECTION ( 'NONE',  ( 0.000000000000000000, 0.000000000000000000, 1.000000000000000000 ) ) ;
#24312 = ORIENTED_EDGE ( 'NONE', *, *, #27371, .T. ) ;
#24313 = AXIS2_PLACEMENT_3D ( 'NONE', #26853, #734, #11740 ) ;
#24314 = CARTESIAN_POINT ( 'NONE',  ( 1.197070535079588716, 0.07874015748031491790, -1.078960298859116707 ) ) ;
#24315 = CARTESIAN_POINT ( 'NONE',  ( 0.7872492035923605025, 0.2535455059636700370, -0.2765862953003382363 ) ) ;
#24316 = CARTESIAN_POINT ( 'NONE',  ( -0.3265485372158890010, -0.1887320510662011952, 0.1992150590373740204 ) ) ;
#24317 = EDGE_CURVE ( 'NONE', #19463, #26623, #4249, .T. ) ;
#24318 = DIRECTION ( 'NONE',  ( 0.000000000000000000, -1.000000000000000000, 0.000000000000000000 ) ) ;
#24319 = DIRECTION ( 'NONE',  ( 0.000000000000000000, 0.000000000000000000, 1.000000000000000000 ) ) ;
#24320 = ORIENTED_EDGE ( 'NONE', *, *, #11733, .F. ) ;
#24321 = CARTESIAN_POINT ( 'NONE',  ( -0.1078280746904044657, 0.3175540113612282389, 1.973425196850393970 ) ) ;
#24322 = CARTESIAN_POINT ( 'NONE',  ( 0.4763861460130704994, -0.1275996891957771051, -1.550196850393700920 ) ) ;
#24323 = EDGE_CURVE ( 'NONE', #17036, #9597, #25221, .T. ) ;
#24324 = CARTESIAN_POINT ( 'NONE',  ( -0.4121342552748326060, -0.2031943647053980340, -1.928289503579156960 ) ) ;
#24325 = AXIS2_PLACEMENT_3D ( 'NONE', #24089, #21702, #19851 ) ;
#24326 = CARTESIAN_POINT ( 'NONE',  ( 0.07214854559196579031, 0.5476281405333208729, 0.9202755905511811330 ) ) ;
#24327 = SPHERICAL_SURFACE ( 'NONE', #1730, 0.1299232283464566984 ) ;
#24328 = EDGE_CURVE ( 'NONE', #8023, #26363, #3305, .T. ) ;
#24329 = CARTESIAN_POINT ( 'NONE',  ( 0.000000000000000000, 0.000000000000000000, 0.07637795275590551769 ) ) ;
#24330 = AXIS2_PLACEMENT_3D ( 'NONE', #21478, #49, #23476 ) ;
#24331 = CARTESIAN_POINT ( 'NONE',  ( 0.3020979083623086536, 0.3591256245825952265, 0.1992125984251968684 ) ) ;
#24332 = CARTESIAN_POINT ( 'NONE',  ( 0.2796934465393868807, 0.3645739570812638330, -1.928289503579156072 ) ) ;
#24333 = B_SPLINE_CURVE_WITH_KNOTS ( 'NONE', 3,
 ( #18196, #11439, #24295, #7484 ),
 .UNSPECIFIED., .F., .F.,
 ( 4, 4 ),
 ( 1.726099910371974966, 1.727746213436275102 ),
 .UNSPECIFIED. ) ;
#24334 = DIRECTION ( 'NONE',  ( 0.000000000000000000, 0.000000000000000000, -1.000000000000000000 ) ) ;
#24335 = CARTESIAN_POINT ( 'NONE',  ( -0.6544535166833030937, -0.006373303606307913032, 0.2362204724409449064 ) ) ;
#24336 = CARTESIAN_POINT ( 'NONE',  ( 0.6299212598425196763, 0.000000000000000000, 0.000000000000000000 ) ) ;
#24337 = CARTESIAN_POINT ( 'NONE',  ( -2.685748425196850164E-17, 0.000000000000000000, -1.894685039405410665 ) ) ;
#24338 = CARTESIAN_POINT ( 'NONE',  ( -0.0006832381873107856631, 0.6614169699452854267, 0.1616495878891046900 ) ) ;
#24339 = DIRECTION ( 'NONE',  ( 0.000000000000000000, 1.000000000000000000, 0.000000000000000000 ) ) ;
#24340 = DIRECTION ( 'NONE',  ( -0.000000000000000000, -1.000000000000000000, -0.000000000000000000 ) ) ;
#24341 = VERTEX_POINT ( 'NONE', #20112 ) ;
#24342 = AXIS2_PLACEMENT_3D ( 'NONE', #17647, #24010, #6240 ) ;
#24343 = CARTESIAN_POINT ( 'NONE',  ( -1.466875984251968630E-17, 0.000000000000000000, 0.000000000000000000 ) ) ;
#24344 = EDGE_CURVE ( 'NONE', #4078, #17378, #9650, .T. ) ;
#24345 = ORIENTED_EDGE ( 'NONE', *, *, #19828, .T. ) ;
#24346 = FACE_OUTER_BOUND ( 'NONE', #12498, .T. ) ;
#24347 = ADVANCED_FACE ( 'NONE', ( #22234 ), #2859, .T. ) ;
#24348 = AXIS2_PLACEMENT_3D ( 'NONE', #15115, #13107, #12964 ) ;
#24349 = DIRECTION ( 'NONE',  ( -0.3420201433256691570, -0.9396926207859082059, 0.000000000000000000 ) ) ;
#24350 = CARTESIAN_POINT ( 'NONE',  ( 0.5905511811023621549, 0.000000000000000000, 0.000000000000000000 ) ) ;
#24351 = DIRECTION ( 'NONE',  ( 0.000000000000000000, 7.180547322999999937E-06, -0.9999999999742198442 ) ) ;
#24352 = DIRECTION ( 'NONE',  ( 0.000000000000000000, 0.000000000000000000, -1.000000000000000000 ) ) ;
#24353 = EDGE_CURVE ( 'NONE', #4182, #11023, #25039, .T. ) ;
#24354 = CIRCLE ( 'NONE', #3150, 0.6212598425196850238 ) ;
#24355 = DIRECTION ( 'NONE',  ( 0.000000000000000000, 1.000000000000000000, 0.000000000000000000 ) ) ;
#24356 = CARTESIAN_POINT ( 'NONE',  ( 0.09762295995069844579, 0.3644697409450269321, -3.100567304031763172 ) ) ;
#24357 = CARTESIAN_POINT ( 'NONE',  ( 0.1181102362204724532, 1.446433227339393765E-17, 0.6228346456772185791 ) ) ;
#24358 = CARTESIAN_POINT ( 'NONE',  ( -0.4339912984563299436, -0.2498791196563492356, 0.09685039370078740717 ) ) ;
#24359 = EDGE_CURVE ( 'NONE', #657, #3526, #3145, .T. ) ;
#24360 = VERTEX_POINT ( 'NONE', #18097 ) ;
#24361 = DIRECTION ( 'NONE',  ( 0.000000000000000000, 0.000000000000000000, -1.000000000000000000 ) ) ;
#24362 = EDGE_CURVE ( 'NONE', #18929, #3892, #16304, .T. ) ;
#24364 = CARTESIAN_POINT ( 'NONE',  ( -0.6912180915490531152, 0.08120084520073209133, -0.2401638807511342344 ) ) ;
#24365 = AXIS2_PLACEMENT_3D ( 'NONE', #14079, #8149, #5896 ) ;
#24366 = EDGE_CURVE ( 'NONE', #15615, #16233, #22334, .T. ) ;
#24367 = DIRECTION ( 'NONE',  ( -3.508908000000002129E-18, 0.5000000000000003331, 0.8660254037844384856 ) ) ;
#24368 = CARTESIAN_POINT ( 'NONE',  ( -0.1771653543307086520, -5.663984251968503442E-18, 0.000000000000000000 ) ) ;
#24369 = CARTESIAN_POINT ( 'NONE',  ( 0.4441657790108421988, 0.2564944395515498798, 1.747047244094488194 ) ) ;
#24370 = EDGE_CURVE ( 'NONE', #27801, #9119, #14047, .T. ) ;
#24371 = ORIENTED_EDGE ( 'NONE', *, *, #14585, .F. ) ;
#24372 = COLOUR_RGB ( '', 0.08235294, 0.09019608, 0.10196078) ;
#24373 = CARTESIAN_POINT ( 'NONE',  ( -0.3726024258163779246, 0.000000000000000000, -3.115157480314960647 ) ) ;
#24374 = EDGE_LOOP ( 'NONE', ( #19237, #17842, #14876, #3736 ) ) ;
#24375 = CARTESIAN_POINT ( 'NONE',  ( 0.7874015748031496509, 0.3326143029362100823, -0.01422925309762631055 ) ) ;
#24376 = CARTESIAN_POINT ( 'NONE',  ( 0.0002199787722797491975, 0.6212598425196850238, 0.09684793308443542803 ) ) ;
#24377 = CARTESIAN_POINT ( 'NONE',  ( 0.2904160862623607620, -0.1677079028045494191, 1.953740157480315043 ) ) ;
#24378 = ORIENTED_EDGE ( 'NONE', *, *, #19409, .F. ) ;
#24379 = ORIENTED_EDGE ( 'NONE', *, *, #20207, .T. ) ;
#24380 = CARTESIAN_POINT ( 'NONE',  ( 0.5511811023622047445, 3.414809992080329023E-17, 0.9202755905511811330 ) ) ;
#24381 = ORIENTED_EDGE ( 'NONE', *, *, #7891, .F. ) ;
#24382 = ORIENTED_EDGE ( 'NONE', *, *, #8243, .F. ) ;
#24383 = ORIENTED_EDGE ( 'NONE', *, *, #7028, .T. ) ;
#24384 = CARTESIAN_POINT ( 'NONE',  ( -0.4527559054764770385, 0.000000000000000000, -1.934055118110236338 ) ) ;
#24385 = CARTESIAN_POINT ( 'NONE',  ( -0.07874015748031511219, 0.1968503937007874127, -3.548228346456693050 ) ) ;
#24386 = CIRCLE ( 'NONE', #27130, 0.3149606299212598381 ) ;
#24387 = DIRECTION ( 'NONE',  ( 0.000000000000000000, 0.000000000000000000, 1.000000000000000000 ) ) ;
#24388 = CARTESIAN_POINT ( 'NONE',  ( -0.4921259842519685179, 3.013402556957069934E-17, -1.569881889763779625 ) ) ;
#24389 = CARTESIAN_POINT ( 'NONE',  ( -0.8725268807032540153, 0.000000000000000000, -1.052618110236220428 ) ) ;
#24390 = CARTESIAN_POINT ( 'NONE',  ( 0.7608910173126012255, 0.6007740188332617581, 0.08763475256689905180 ) ) ;
#24391 = ADVANCED_FACE ( 'NONE', ( #770 ), #17964, .F. ) ;
#24392 = AXIS2_PLACEMENT_3D ( 'NONE', #24784, #26764, #1211 ) ;
#24393 = CARTESIAN_POINT ( 'NONE',  ( 1.197070535079588716, 0.07874015748031491790, 1.078960298859116707 ) ) ;
#24394 = CARTESIAN_POINT ( 'NONE',  ( 0.6342142812972784149, 0.1111449751016729826, 0.1183902030411032036 ) ) ;
#24395 = CARTESIAN_POINT ( 'NONE',  ( 0.7874015748031496509, -0.3839064563524838825, -0.3321176343386787466 ) ) ;
#24396 = DIRECTION ( 'NONE',  ( 0.2036417511401770464, 0.4895227362422922002, 0.8478782506317882328 ) ) ;
#24397 = ( REPRESENTATION_RELATIONSHIP ('NONE','NONE', #12434, #16232 ) REPRESENTATION_RELATIONSHIP_WITH_TRANSFORMATION ( #21029 )SHAPE_REPRESENTATION_RELATIONSHIP( ) ) ;
#24398 = DIRECTION ( 'NONE',  ( 0.000000000000000000, 0.000000000000000000, -1.000000000000000000 ) ) ;
#24399 = CARTESIAN_POINT ( 'NONE',  ( 0.4612490782035170156, 0.2663596103035609786, 1.747047244094488194 ) ) ;
#24400 = APPLICATION_CONTEXT ( 'automotive_design' ) ;
#24401 = ORIENTED_EDGE ( 'NONE', *, *, #15982, .T. ) ;
#24402 = VECTOR ( 'NONE', #5715, 39.37007874015748854 ) ;
#24403 = CARTESIAN_POINT ( 'NONE',  ( 0.07874015748031495954, -0.04546065111729338803, -0.4724409448818898127 ) ) ;
#24404 = ORIENTED_EDGE ( 'NONE', *, *, #21282, .T. ) ;
#24405 = DIRECTION ( 'NONE',  ( 0.000000000000000000, -0.8660254037844384856, 0.5000000000000003331 ) ) ;
#24406 = EDGE_LOOP ( 'NONE', ( #10902, #3557, #6730, #11078 ) ) ;
#24407 = CARTESIAN_POINT ( 'NONE',  ( -0.5379714048901780288, 0.000000000000000000, -0.2480314960629921295 ) ) ;
#24408 = AXIS2_PLACEMENT_3D ( 'NONE', #22169, #5064, #26528 ) ;
#24409 = ORIENTED_EDGE ( 'NONE', *, *, #17691, .F. ) ;
#24410 = AXIS2_PLACEMENT_3D ( 'NONE', #14351, #3439, #25637 ) ;
#24411 = CARTESIAN_POINT ( 'NONE',  ( 0.1275996891957681401, 0.4763861460130344172, -1.569881889763779625 ) ) ;
#24412 = DIRECTION ( 'NONE',  ( 1.000000000000000000, 0.000000000000000000, 0.000000000000000000 ) ) ;
#24413 = AXIS2_PLACEMENT_3D ( 'NONE', #1012, #26560, #5091 ) ;
#24414 = ORIENTED_EDGE ( 'NONE', *, *, #17696, .T. ) ;
#24415 = CARTESIAN_POINT ( 'NONE',  ( 0.3362148458988509225, -0.4382482975804891101, 0.9399606299212598381 ) ) ;
#24416 = CARTESIAN_POINT ( 'NONE',  ( 0.09590060490395689585, -0.1136516277932334562, 0.1968503937007874127 ) ) ;
#24417 = ADVANCED_FACE ( 'NONE', ( #22655 ), #18537, .F. ) ;
#24418 = DIMENSIONAL_EXPONENTS ( 1.000000000000000000, 0.000000000000000000, 0.000000000000000000, 0.000000000000000000, 0.000000000000000000, 0.000000000000000000, 0.000000000000000000 ) ;
#24419 = CARTESIAN_POINT ( 'NONE',  ( 0.3464566929133857665, 0.000000000000000000, 0.1377952755905511584 ) ) ;
#24420 = FACE_OUTER_BOUND ( 'NONE', #1242, .T. ) ;
#24421 = DIRECTION ( 'NONE',  ( 0.000000000000000000, 0.000000000000000000, 1.000000000000000000 ) ) ;
#24422 = B_SPLINE_CURVE_WITH_KNOTS ( 'NONE', 3,
 ( #11821, #14085, #18009, #20441, #22702, #18582 ),
 .UNSPECIFIED., .F., .F.,
 ( 4, 2, 4 ),
 ( 1.162880698919835920, 1.164573402063409979, 1.166266105206986037 ),
 .UNSPECIFIED. ) ;
#24423 = EDGE_CURVE ( 'NONE', #18589, #5007, #5486, .T. ) ;
#24424 = EDGE_CURVE ( 'NONE', #12685, #10034, #10532, .T. ) ;
#24425 = VECTOR ( 'NONE', #21100, 39.37007874015748143 ) ;
#24426 = CARTESIAN_POINT ( 'NONE',  ( 0.5869493968219645641, 0.4267795243146149664, 0.000000000000000000 ) ) ;
#24427 = DIRECTION ( 'NONE',  ( -7.017815000000000124E-18, 1.000000000000000000, -1.224646799147353207E-16 ) ) ;
#24428 = MECHANICAL_DESIGN_GEOMETRIC_PRESENTATION_REPRESENTATION (  '', ( #14057 ), #21290 ) ;
#24429 = CIRCLE ( 'NONE', #12264, 0.1673228346456692994 ) ;
#24430 = LINE ( 'NONE', #15968, #6285 ) ;
#24431 = CARTESIAN_POINT ( 'NONE',  ( 0.2078289949484099508, -0.4330237525398077936, 0.2362204724409449619 ) ) ;
#24432 = DIRECTION ( 'NONE',  ( 0.000000000000000000, 0.000000000000000000, -1.000000000000000000 ) ) ;
#24433 = DIRECTION ( 'NONE',  ( 0.7212949172625979788, 8.833315116668955568E-17, -0.6926280692631088254 ) ) ;
#24434 = CYLINDRICAL_SURFACE ( 'NONE', #21454, 0.1181102362204718703 ) ;
#24435 = AXIS2_PLACEMENT_3D ( 'NONE', #26437, #21794, #19399 ) ;
#24436 = CARTESIAN_POINT ( 'NONE',  ( -0.7165354330708662012, 8.775028245858987528E-17, 0.3425196850393700809 ) ) ;
#24437 = CARTESIAN_POINT ( 'NONE',  ( -1.197070535079588716, 0.07874015748031495954, -1.315180771300060503 ) ) ;
#24438 = ORIENTED_EDGE ( 'NONE', *, *, #24132, .T. ) ;
#24439 = CIRCLE ( 'NONE', #11208, 0.8267716535433071723 ) ;
#24440 = VERTEX_POINT ( 'NONE', #1592 ) ;
#24441 = AXIS2_PLACEMENT_3D ( 'NONE', #8836, #12526, #25377 ) ;
#24442 = CARTESIAN_POINT ( 'NONE',  ( -0.07874015748031495954, -1.062017969535966354E-23, -0.4653543306978102367 ) ) ;
#24443 = CARTESIAN_POINT ( 'NONE',  ( 0.000000000000000000, 0.000000000000000000, 0.4488188976377953110 ) ) ;
#24444 = CARTESIAN_POINT ( 'NONE',  ( 0.7430739993161732393, 0.4449930158387386259, -0.3601246575843464748 ) ) ;
#24445 = AXIS2_PLACEMENT_3D ( 'NONE', #21419, #14521, #8419 ) ;
#24446 = EDGE_CURVE ( 'NONE', #13062, #14040, #14172, .T. ) ;
#24447 = ORIENTED_EDGE ( 'NONE', *, *, #5950, .T. ) ;
#24448 = CARTESIAN_POINT ( 'NONE',  ( 0.2564944395535760924, 0.4441657790094617475, -1.550196850393700920 ) ) ;
#24449 = AXIS2_PLACEMENT_3D ( 'NONE', #4985, #6712, #17435 ) ;
#24450 = CARTESIAN_POINT ( 'NONE',  ( 0.06001958459474798779, 0.4555658499976080189, -1.928289503579158515 ) ) ;
#24451 = AXIS2_PLACEMENT_3D ( 'NONE', #9165, #1679, #22883 ) ;
#24452 = CARTESIAN_POINT ( 'NONE',  ( 0.6397637795275591399, 0.000000000000000000, 0.000000000000000000 ) ) ;
#24453 = CARTESIAN_POINT ( 'NONE',  ( -0.4954197419817713000, -0.2442565704126117565, 0.9202755905511811330 ) ) ;
#24454 = CARTESIAN_POINT ( 'NONE',  ( 0.6117062799105531523, 0.1085321106658064944, 0.2574803149606298969 ) ) ;
#24455 = CARTESIAN_POINT ( 'NONE',  ( 0.1247869790670923795, -0.3443449118002068210, 0.08455817587526011370 ) ) ;
#24456 = CARTESIAN_POINT ( 'NONE',  ( 0.000000000000000000, 0.5007874015748031704, 0.04842519685039370358 ) ) ;
#24457 = ADVANCED_BREP_SHAPE_REPRESENTATION ( 'ISO 4762 M5x16 Socket Head Cap Screw', ( #21926, #11588 ), #3473 ) ;
#24458 = CARTESIAN_POINT ( 'NONE',  ( -0.2466292688015201129, 0.4270824798167635050, -1.569881889763779625 ) ) ;
#24459 = CARTESIAN_POINT ( 'NONE',  ( 0.4858607088160724063, -0.2805118110236220486, 0.1771653543307086520 ) ) ;
#24460 = DIRECTION ( 'NONE',  ( -1.000000000000000000, 0.000000000000000000, 0.000000000000000000 ) ) ;
#24461 = DIRECTION ( 'NONE',  ( 0.000000000000000000, 0.000000000000000000, -1.000000000000000000 ) ) ;
#24462 = EDGE_CURVE ( 'NONE', #3117, #4205, #19136, .T. ) ;
#24463 = EDGE_CURVE ( 'NONE', #10706, #14762, #18222, .T. ) ;
#24464 = PRODUCT_DEFINITION ( 'UNKNOWN', '', #15202, #3157 ) ;
#24465 = CARTESIAN_POINT ( 'NONE',  ( -0.2362204724409449064, -0.4724409448818898127, 0.9491381768041928790 ) ) ;
#24466 = B_SPLINE_CURVE_WITH_KNOTS ( 'NONE', 3,
 ( #23010, #18456, #1116, #12401, #12255, #11981 ),
 .UNSPECIFIED., .F., .F.,
 ( 4, 2, 4 ),
 ( 0.5000000000000000000, 0.7500000000000000000, 1.000000000000000000 ),
 .UNSPECIFIED. ) ;
#24467 = PRODUCT_DEFINITION_SHAPE ( 'NONE', 'NONE',  #27885 ) ;
#24468 = CARTESIAN_POINT ( 'NONE',  ( -0.1189624676717059848, -0.3253923344978159604, 0.1377952755905513249 ) ) ;
#24469 = EDGE_CURVE ( 'NONE', #23967, #13155, #11922, .T. ) ;
#24470 = ORIENTED_EDGE ( 'NONE', *, *, #19376, .F. ) ;
#24471 = AXIS2_PLACEMENT_3D ( 'NONE', #6956, #1559, #18781 ) ;
#24472 = CARTESIAN_POINT ( 'NONE',  ( 0.2161891097063337874, 0.2816986811834100157, 1.953740157480314599 ) ) ;
#24473 = ORIENTED_EDGE ( 'NONE', *, *, #24868, .F. ) ;
#24474 = CARTESIAN_POINT ( 'NONE',  ( -0.1458850421962728516, -0.4296318976990441407, -1.934055118110236338 ) ) ;
#24475 = AXIS2_PLACEMENT_3D ( 'NONE', #22103, #14711, #10816 ) ;
#24476 = CARTESIAN_POINT ( 'NONE',  ( -0.07217847769028858107, -0.04546065111729339497, -5.567324087794789421E-18 ) ) ;
#24477 = CARTESIAN_POINT ( 'NONE',  ( 2.632951206231566310, -0.4724409448818898127, 0.8182917201112794858 ) ) ;
#24478 = CARTESIAN_POINT ( 'NONE',  ( 0.1493295869868995762, -0.2561000767422981772, -0.4059580611872550260 ) ) ;
#24479 = EDGE_CURVE ( 'NONE', #7932, #8591, #9196, .T. ) ;
#24480 = ADVANCED_FACE ( 'NONE', ( #25610 ), #23230, .F. ) ;
#24481 = EDGE_LOOP ( 'NONE', ( #17205, #12263 ) ) ;
#24482 = DIRECTION ( 'NONE',  ( 0.000000000000000000, 0.000000000000000000, -1.000000000000000000 ) ) ;
#24483 = DIRECTION ( 'NONE',  ( -1.000000000000000000, 0.000000000000000000, 0.000000000000000000 ) ) ;
#24484 = DIRECTION ( 'NONE',  ( 0.000000000000000000, 0.000000000000000000, -1.000000000000000000 ) ) ;
#24485 = AXIS2_PLACEMENT_3D ( 'NONE', #6944, #4797, #15566 ) ;
#24486 = DIRECTION ( 'NONE',  ( -0.9749279121818237304, -0.2225209339563138378, 0.000000000000000000 ) ) ;
#24487 = CARTESIAN_POINT ( 'NONE',  ( -0.09762295995069376897, -0.3644697409450285974, -3.100567304031760951 ) ) ;
#24488 = DIRECTION ( 'NONE',  ( 0.000000000000000000, 0.000000000000000000, 1.000000000000000000 ) ) ;
#24489 = ORIENTED_EDGE ( 'NONE', *, *, #15884, .T. ) ;
#24490 = CARTESIAN_POINT ( 'NONE',  ( -0.2228126397719833174, 0.3858397471888795893, -1.934055118110236338 ) ) ;
#24491 = B_SPLINE_CURVE_WITH_KNOTS ( 'NONE', 3,
 ( #27415, #19351, #7924, #8350, #6098, #1975 ),
 .UNSPECIFIED., .F., .F.,
 ( 4, 2, 4 ),
 ( 0.2291966065698869959, 0.2305109203526909956, 0.2318252341354939960 ),
 .UNSPECIFIED. ) ;
#24492 = CARTESIAN_POINT ( 'NONE',  ( -0.2031943647053778002, -0.4121342552748231136, -1.928289503579173614 ) ) ;
#24493 = CARTESIAN_POINT ( 'NONE',  ( -0.7121770198535963825, 0.1302456093167436990, -0.2464793285356193242 ) ) ;
#24494 = AXIS2_PLACEMENT_3D ( 'NONE', #22341, #11601, #3245 ) ;
#24495 = VERTEX_POINT ( 'NONE', #1452 ) ;
#24496 = CARTESIAN_POINT ( 'NONE',  ( -0.3503688343903059166, -0.8773679034442795066, -0.6250144544381456280 ) ) ;
#24497 = DIRECTION ( 'NONE',  ( 0.000000000000000000, 0.000000000000000000, 1.000000000000000000 ) ) ;
#24498 = CARTESIAN_POINT ( 'NONE',  ( -0.4954415918530866159, 0.1327036767659691974, 1.747047244094488194 ) ) ;
#24499 = ORIENTED_EDGE ( 'NONE', *, *, #9608, .F. ) ;
#24500 = ADVANCED_FACE ( 'NONE', ( #27598 ), #2454, .T. ) ;
#24501 = VECTOR ( 'NONE', #24668, 39.37007874015748143 ) ;
#24502 = CARTESIAN_POINT ( 'NONE',  ( -0.2836590635674538508, 0.2488091035917008864, -3.100567304031763172 ) ) ;
#24503 = EDGE_CURVE ( 'NONE', #7615, #15934, #20490, .T. ) ;
#24504 = AXIS2_PLACEMENT_3D ( 'NONE', #13989, #22594, #16248 ) ;
#24505 = ORIENTED_EDGE ( 'NONE', *, *, #19686, .T. ) ;
#24506 = CARTESIAN_POINT ( 'NONE',  ( -0.6251768273491621342, 1.092930385926066394, -0.09774754414306212336 ) ) ;
#24507 = CARTESIAN_POINT ( 'NONE',  ( 0.1495939273659337154, 0.2606208377493157702, -0.4045036076671820746 ) ) ;
#24508 = EDGE_CURVE ( 'NONE', #11010, #24104, #16586, .T. ) ;
#24509 = VERTEX_POINT ( 'NONE', #5988 ) ;
#24510 = EDGE_LOOP ( 'NONE', ( #16052, #9656, #1125, #16484 ) ) ;
#24511 = CARTESIAN_POINT ( 'NONE',  ( -0.3693533223127509202, -0.6818538191143146410, -0.6013702642917986285 ) ) ;
#24512 = VERTEX_POINT ( 'NONE', #12473 ) ;
#24513 = DIRECTION ( 'NONE',  ( 1.000000000000000000, 0.000000000000000000, 0.000000000000000000 ) ) ;
#24514 = EDGE_CURVE ( 'NONE', #26492, #16539, #26816, .T. ) ;
#24515 = VERTEX_POINT ( 'NONE', #12616 ) ;
#24516 = CARTESIAN_POINT ( 'NONE',  ( 0.02909913904662007542, 0.4446020952038907681, -1.934055118110236338 ) ) ;
#24517 = VERTEX_POINT ( 'NONE', #18667 ) ;
#24518 = EDGE_LOOP ( 'NONE', ( #21645, #6760, #4716, #7713, #8699, #19669 ) ) ;
#24519 = CARTESIAN_POINT ( 'NONE',  ( -0.2965233727166468047, 0.3524965443697193335, 0.1771653543307085965 ) ) ;
#24520 = DIRECTION ( 'NONE',  ( 0.000000000000000000, 0.000000000000000000, 1.000000000000000000 ) ) ;
#24521 = CIRCLE ( 'NONE', #23199, 0.1308464566929133932 ) ;
#24522 = CARTESIAN_POINT ( 'NONE',  ( 0.3843128886798078958, 0.1965195625994889950, 0.07874015748031495954 ) ) ;
#24523 = CARTESIAN_POINT ( 'NONE',  ( -0.3105958729522376172, -0.6467467715313297560, 0.1601585119463167506 ) ) ;
#24524 = LINE ( 'NONE', #20295, #23675 ) ;
#24525 = EDGE_CURVE ( 'NONE', #3577, #15134, #18676, .T. ) ;
#24526 = AXIS2_PLACEMENT_3D ( 'NONE', #20233, #749, #9338 ) ;
#24527 = CARTESIAN_POINT ( 'NONE',  ( -1.692913385826771533, 0.07874015748031495954, -1.036610629921259805E-16 ) ) ;
#24528 = CARTESIAN_POINT ( 'NONE',  ( 0.3346456692913385433, -0.04380501567505458438, 1.973425196850393526 ) ) ;
#24529 = AXIS2_PLACEMENT_3D ( 'NONE', #10152, #1686, #8193 ) ;
#24530 = CARTESIAN_POINT ( 'NONE',  ( -0.2161381151962937508, 0.2817310484609270027, 1.953740157480315043 ) ) ;
#24531 = DIRECTION ( 'NONE',  ( 0.000000000000000000, 0.000000000000000000, -1.000000000000000000 ) ) ;
#24532 = CARTESIAN_POINT ( 'NONE',  ( 0.000000000000000000, 0.000000000000000000, -0.2480314960629921295 ) ) ;
#24533 = CARTESIAN_POINT ( 'NONE',  ( -1.928513779527558736E-17, 0.000000000000000000, -0.03543307086614173179 ) ) ;
#24534 = DIRECTION ( 'NONE',  ( 1.000000000000000000, 0.000000000000000000, 0.000000000000000000 ) ) ;
#24535 = CARTESIAN_POINT ( 'NONE',  ( 0.4069448477556011912, 0.3121994997598430133, 1.766732283464566899 ) ) ;
#24536 = AXIS2_PLACEMENT_3D ( 'NONE', #21881, #24398, #13255 ) ;
#24537 = EDGE_LOOP ( 'NONE', ( #15027, #21310 ) ) ;
#24538 = EDGE_CURVE ( 'NONE', #21208, #19384, #14194, .T. ) ;
#24539 = CARTESIAN_POINT ( 'NONE',  ( 0.03008364706454716778, -0.1136516277932324709, -0.1968503937007874127 ) ) ;
#24540 = LINE ( 'NONE', #5343, #17726 ) ;
#24541 = EDGE_CURVE ( 'NONE', #15200, #3726, #17354, .T. ) ;
#24542 = ORIENTED_EDGE ( 'NONE', *, *, #10729, .F. ) ;
#24543 = DIRECTION ( 'NONE',  ( 0.000000000000000000, 1.000000000000000000, 0.000000000000000000 ) ) ;
#24544 = CIRCLE ( 'NONE', #7897, 0.08582677165167480748 ) ;
#24545 = CARTESIAN_POINT ( 'NONE',  ( 0.3001918266902144361, -0.3912931228432220410, -1.569881889763779625 ) ) ;
#24546 = CARTESIAN_POINT ( 'NONE',  ( 0.2720459371704843088, 0.3242117229735830830, 0.2145688976377952695 ) ) ;
#24547 = AXIS2_PLACEMENT_3D ( 'NONE', #19104, #20669, #18529 ) ;
#24548 = ORIENTED_EDGE ( 'NONE', *, *, #23839, .F. ) ;
#24549 = ORIENTED_EDGE ( 'NONE', *, *, #24328, .T. ) ;
#24550 = CARTESIAN_POINT ( 'NONE',  ( 0.4152525734086595088, -0.3642352168757885811, 0.9399606299212598381 ) ) ;
#24551 = ORIENTED_EDGE ( 'NONE', *, *, #12405, .T. ) ;
#24552 = EDGE_CURVE ( 'NONE', #24279, #24109, #5145, .T. ) ;
#24553 = CYLINDRICAL_SURFACE ( 'NONE', #17143, 0.1771653543307086520 ) ;
#24554 = DIRECTION ( 'NONE',  ( -0.2036417511401762415, -0.4895227362422910344, 0.8478782506317890100 ) ) ;
#24555 = CARTESIAN_POINT ( 'NONE',  ( -0.1771653543307086520, -5.663984251968503442E-18, 0.000000000000000000 ) ) ;
#24556 = PLANE ( 'NONE',  #18834 ) ;
#24557 = CARTESIAN_POINT ( 'NONE',  ( 0.000000000000000000, 0.000000000000000000, 0.1992125984251968684 ) ) ;
#24558 = CARTESIAN_POINT ( 'NONE',  ( -0.4621283342336243716, 0.08168108835551378399, 0.1992150590373740204 ) ) ;
#24559 = CARTESIAN_POINT ( 'NONE',  ( 0.000000000000000000, 0.000000000000000000, 0.1992125984251968684 ) ) ;
#24560 = EDGE_CURVE ( 'NONE', #21933, #724, #16428, .T. ) ;
#24561 = B_SPLINE_CURVE_WITH_KNOTS ( 'NONE', 3,
 ( #939, #24506, #5156, #22402, #5303, #18127, #7418, #14069, #11800, #22681, #16192 ),
 .UNSPECIFIED., .F., .F.,
 ( 4, 2, 1, 2, 2, 4 ),
 ( 0.000000000000000000, 0.1250000000000002220, 0.1875000000000006661, 0.2187500000000006384, 0.2500000000000006106, 0.5000000000000000000 ),
 .UNSPECIFIED. ) ;
#24562 = LINE ( 'NONE', #9736, #5106 ) ;
#24563 = CONTEXT_DEPENDENT_SHAPE_REPRESENTATION ( #13071, #17916 ) ;
#24564 = CARTESIAN_POINT ( 'NONE',  ( 0.2660793235464290474, -0.2041304421298306693, 1.953740157480315043 ) ) ;
#24565 = UNCERTAINTY_MEASURE_WITH_UNIT (LENGTH_MEASURE( 1.000000000000000082E-05 ), #17236, 'distance_accuracy_value', 'NONE') ;
#24566 = ORIENTED_EDGE ( 'NONE', *, *, #7949, .T. ) ;
#24567 = CARTESIAN_POINT ( 'NONE',  ( 0.1198326771653543399, -1.315836188112322458E-17, -0.1074461786882927178 ) ) ;
#24568 = CARTESIAN_POINT ( 'NONE',  ( -0.5905511811023621549, 0.000000000000000000, 0.000000000000000000 ) ) ;
#24569 = CIRCLE ( 'NONE', #17806, 1.377952755905512472 ) ;
#24570 = CARTESIAN_POINT ( 'NONE',  ( -0.6385905051800526699, -0.06366962376380753963, 0.2346802187740419654 ) ) ;
#24571 = CARTESIAN_POINT ( 'NONE',  ( 0.1608692170994283632, -0.4408576787418519993, 0.1992142434433712694 ) ) ;
#24572 = TOROIDAL_SURFACE ( 'NONE', #10584, 0.1476377952755905387, 0.01968503937007873988 ) ;
#24573 = CARTESIAN_POINT ( 'NONE',  ( -5.645730259564185549E-17, 0.4692913385826772976, 0.07637549214372836570 ) ) ;
#24574 = CARTESIAN_POINT ( 'NONE',  ( -0.3874223757850451810, 0.3097832252386399365, 0.1734435147365480934 ) ) ;
#24575 = DIRECTION ( 'NONE',  ( -0.4999999999999993894, 0.000000000000000000, -0.8660254037844389297 ) ) ;
#24576 = DIRECTION ( 'NONE',  ( 1.000000000000000000, 0.000000000000000000, 0.000000000000000000 ) ) ;
#24577 = EDGE_CURVE ( 'NONE', #8473, #4752, #15116, .T. ) ;
#24578 = EDGE_CURVE ( 'NONE', #8859, #13133, #12387, .T. ) ;
#24579 = AXIS2_PLACEMENT_3D ( 'NONE', #11514, #393, #17597 ) ;
#24580 = EDGE_LOOP ( 'NONE', ( #19668, #22109, #8453, #25361, #12213, #25290 ) ) ;
#24581 = DIRECTION ( 'NONE',  ( 0.000000000000000000, 1.000000000000000000, 0.000000000000000000 ) ) ;
#24582 = CARTESIAN_POINT ( 'NONE',  ( -0.3197948809234547607, -0.6622502000709752368, 0.2763636194350204134 ) ) ;
#24583 = CARTESIAN_POINT ( 'NONE',  ( 0.07870736599822261703, 0.1968503937007382021, -3.608715228723502921 ) ) ;
#24584 = CARTESIAN_POINT ( 'NONE',  ( -0.5118110236220473341, 0.03361326524566096707, -1.550196850393701142 ) ) ;
#24585 = CARTESIAN_POINT ( 'NONE',  ( -0.09139240964747703810, 0.07874015748031500117, 0.02109836160874967170 ) ) ;
#24586 = ORIENTED_EDGE ( 'NONE', *, *, #19573, .F. ) ;
#24587 = CIRCLE ( 'NONE', #9713, 0.4941010236220472751 ) ;
#24588 = AXIS2_PLACEMENT_3D ( 'NONE', #12197, #6516, #15146 ) ;
#24589 = DIRECTION ( 'NONE',  ( 0.000000000000000000, 0.000000000000000000, 1.000000000000000000 ) ) ;
#24590 = CARTESIAN_POINT ( 'NONE',  ( 0.7430739993161732393, 0.4441346409226165082, -0.3614604744752461518 ) ) ;
#24591 = EDGE_CURVE ( 'NONE', #6591, #26289, #11706, .T. ) ;
#24592 = DIRECTION ( 'NONE',  ( 0.8571673003991039375, 1.049727190767540375E-16, -0.5150380754143447648 ) ) ;
#24593 = EDGE_LOOP ( 'NONE', ( #27205, #20246, #25675, #9229 ) ) ;
#24594 = CARTESIAN_POINT ( 'NONE',  ( -0.2041304421298429650, -0.2660793235464223860, 1.973425196850393970 ) ) ;
#24595 = CARTESIAN_POINT ( 'NONE',  ( -0.2180862235769588653, -0.4423390553432484107, -1.550196850393700920 ) ) ;
#24596 = AXIS2_PLACEMENT_3D ( 'NONE', #24138, #17765, #19898 ) ;
#24597 = CARTESIAN_POINT ( 'NONE',  ( -0.1294857240059045234, -0.3542416573274181357, 0.1992125984251968684 ) ) ;
#24598 = DIRECTION ( 'NONE',  ( 0.000000000000000000, 0.000000000000000000, 1.000000000000000000 ) ) ;
#24599 = DIRECTION ( 'NONE',  ( 0.000000000000000000, 0.000000000000000000, 1.000000000000000000 ) ) ;
#24600 = CARTESIAN_POINT ( 'NONE',  ( -0.3937007874015748254, 4.966087413865251393E-17, 0.02362204724409448786 ) ) ;
#24601 = ( REPRESENTATION_RELATIONSHIP ('NONE','NONE', #12434, #713 ) REPRESENTATION_RELATIONSHIP_WITH_TRANSFORMATION ( #21740 )SHAPE_REPRESENTATION_RELATIONSHIP( ) ) ;
#24602 = FACE_OUTER_BOUND ( 'NONE', #6059, .T. ) ;
#24603 = AXIS2_PLACEMENT_3D ( 'NONE', #23917, #83, #4421 ) ;
#24604 = DIRECTION ( 'NONE',  ( 0.7660444431189780135, 0.6427876096865392519, 0.000000000000000000 ) ) ;
#24605 = CARTESIAN_POINT ( 'NONE',  ( 0.2979095355689177493, -0.6203660015065670663, 0.3401574803149606252 ) ) ;
#24606 = DIRECTION ( 'NONE',  ( 1.000000000000000000, 0.000000000000000000, 0.000000000000000000 ) ) ;
#24607 = ADVANCED_FACE ( 'NONE', ( #20370, #15998 ), #14168, .T. ) ;
#24608 = ORIENTED_EDGE ( 'NONE', *, *, #10017, .F. ) ;
#24609 = ( CONVERSION_BASED_UNIT ( 'INCH', #21720 ) LENGTH_UNIT ( ) NAMED_UNIT ( #16506 ) ) ;
#24610 = DIRECTION ( 'NONE',  ( 0.000000000000000000, 0.000000000000000000, 1.000000000000000000 ) ) ;
#24611 = CYLINDRICAL_SURFACE ( 'NONE', #11399, 0.3346456692913385988 ) ;
#24612 = ORIENTED_EDGE ( 'NONE', *, *, #18615, .T. ) ;
#24613 = CARTESIAN_POINT ( 'NONE',  ( -0.1570773243922992946, 0.3184597017669829055, 1.953740157480315043 ) ) ;
#24614 = ORIENTED_EDGE ( 'NONE', *, *, #14718, .T. ) ;
#24615 = ORIENTED_EDGE ( 'NONE', *, *, #10010, .F. ) ;
#24616 = CARTESIAN_POINT ( 'NONE',  ( -0.3411003281197191872, -0.2991932138496762317, -1.934055118110236338 ) ) ;
#24617 = DIRECTION ( 'NONE',  ( 0.000000000000000000, 1.000000000000000000, 0.000000000000000000 ) ) ;
#24618 = DIRECTION ( 'NONE',  ( 0.000000000000000000, 0.000000000000000000, 1.000000000000000000 ) ) ;
#24619 = CARTESIAN_POINT ( 'NONE',  ( 0.006559182411507800264, 0.3149605050255358529, -3.174212998091514137 ) ) ;
#24620 = DIRECTION ( 'NONE',  ( 0.000000000000000000, -1.000000000000000000, 0.000000000000000000 ) ) ;
#24621 = CARTESIAN_POINT ( 'NONE',  ( 0.03008364706454716778, 0.1136516277932340530, -0.1968503937007874127 ) ) ;
#24622 = VERTEX_POINT ( 'NONE', #9770 ) ;
#24623 = CARTESIAN_POINT ( 'NONE',  ( -0.2223167940359792594, 0.2657206863494902538, 0.1377952755905513249 ) ) ;
#24624 = CARTESIAN_POINT ( 'NONE',  ( -0.3995913070739969819, -0.1970988029421826826, -1.934055118110236338 ) ) ;
#24625 = CARTESIAN_POINT ( 'NONE',  ( 0.3644697409450285974, -0.09762295995069371346, -3.100567304031760951 ) ) ;
#24626 = TOROIDAL_SURFACE ( 'NONE', #21489, 0.5610236220472440971, 0.1003937007874015908 ) ;
#24627 = CARTESIAN_POINT ( 'NONE',  ( 0.0005939837304750000086, 0.5007870493127504208, 0.09685039370078740717 ) ) ;
#24628 = ORIENTED_EDGE ( 'NONE', *, *, #5878, .T. ) ;
#24629 = EDGE_CURVE ( 'NONE', #4795, #12305, #11039, .T. ) ;
#24630 = CARTESIAN_POINT ( 'NONE',  ( 0.3996230174612959707, 0.1970259548082022305, -1.934055118110236338 ) ) ;
#24631 = AXIS2_PLACEMENT_3D ( 'NONE', #7681, #17956, #26731 ) ;
#24632 = CARTESIAN_POINT ( 'NONE',  ( -0.3645739570812778219, -0.2796934465393718927, -1.928289503579152742 ) ) ;
#24633 = LINE ( 'NONE', #12353, #7643 ) ;
#24634 = ORIENTED_EDGE ( 'NONE', *, *, #2372, .F. ) ;
#24635 = EDGE_CURVE ( 'NONE', #10511, #10256, #7411, .T. ) ;
#24636 = CARTESIAN_POINT ( 'NONE',  ( -0.3338887748335567229, -0.7967198305134626235, -0.8696351319825925685 ) ) ;
#24637 = CARTESIAN_POINT ( 'NONE',  ( 0.000000000000000000, 0.9055118110236221041, 0.000000000000000000 ) ) ;
#24638 = CARTESIAN_POINT ( 'NONE',  ( -0.4441657790107820802, -0.2564944395515947884, 1.747047244094488194 ) ) ;
#24639 = VERTEX_POINT ( 'NONE', #11036 ) ;
#24640 = DIRECTION ( 'NONE',  ( -0.2036417511401758251, -0.4895227362422921447, -0.8478782506317885659 ) ) ;
#24641 = VERTEX_POINT ( 'NONE', #72 ) ;
#24642 = AXIS2_PLACEMENT_3D ( 'NONE', #18911, #14984, #19197 ) ;
#24643 = AXIS2_PLACEMENT_3D ( 'NONE', #2259, #2130, #18675 ) ;
#24644 = ORIENTED_EDGE ( 'NONE', *, *, #26777, .F. ) ;
#24645 = CARTESIAN_POINT ( 'NONE',  ( 0.003937007874015826907, -0.09842519685039370636, 1.205361022782828035E-17 ) ) ;
#24646 = CARTESIAN_POINT ( 'NONE',  ( 0.09590060490395689585, 0.1136516277932334562, 0.1968503937007874127 ) ) ;
#24647 = EDGE_LOOP ( 'NONE', ( #4849, #5348, #3983, #6613, #25488, #20786 ) ) ;
#24648 = ORIENTED_EDGE ( 'NONE', *, *, #3494, .T. ) ;
#24649 = CIRCLE ( 'NONE', #3453, 0.4055118110236220486 ) ;
#24650 = CARTESIAN_POINT ( 'NONE',  ( 0.000000000000000000, 0.4724409448818898127, -1.692913385826771533 ) ) ;
#24651 = DIRECTION ( 'NONE',  ( -0.5000000010362850578, 0.8660254031861391866, 0.000000000000000000 ) ) ;
#24652 = ORIENTED_EDGE ( 'NONE', *, *, #20995, .F. ) ;
#24653 = EDGE_LOOP ( 'NONE', ( #5783, #12767 ) ) ;
#24654 = CARTESIAN_POINT ( 'NONE',  ( 0.0005939837304750000086, 0.5007870493127504208, 0.2574803149606298969 ) ) ;
#24655 = CARTESIAN_POINT ( 'NONE',  ( 0.4898768902087983768, 0.000000000000000000, -0.2362204724409449064 ) ) ;
#24656 = CARTESIAN_POINT ( 'NONE',  ( 0.07874015748031489015, 0.1968503937007874127, -3.272637795275590733 ) ) ;
#24657 = CYLINDRICAL_SURFACE ( 'NONE', #9836, 1.288838582677165556 ) ;
#24658 = DIRECTION ( 'NONE',  ( -0.9790454724845842893, -0.2036417511401760472, 2.493892000000000781E-17 ) ) ;
#24659 = CARTESIAN_POINT ( 'NONE',  ( -0.2490711204941342405, 1.060861271878683176, -0.6594961294738858060 ) ) ;
#24660 = ADVANCED_FACE ( 'NONE', ( #12290 ), #12059, .F. ) ;
#24661 = DIRECTION ( 'NONE',  ( 0.000000000000000000, 0.000000000000000000, 1.000000000000000000 ) ) ;
#24662 = LINE ( 'NONE', #3765, #16217 ) ;
#24663 = ADVANCED_FACE ( 'NONE', ( #11306 ), #18561, .F. ) ;
#24664 = CARTESIAN_POINT ( 'NONE',  ( 0.6514872030416209991, 0.1141809932448827059, 0.1926811207754475230 ) ) ;
#24665 = CARTESIAN_POINT ( 'NONE',  ( -0.3362336590883616139, -0.1141709026133614219, 1.953740157480315043 ) ) ;
#24666 = ADVANCED_FACE ( 'NONE', ( #21695, #17311 ), #27779, .T. ) ;
#24667 = ORIENTED_EDGE ( 'NONE', *, *, #6377, .F. ) ;
#24668 = DIRECTION ( 'NONE',  ( -0.000000000000000000, -1.000000000000000000, -0.000000000000000000 ) ) ;
#24669 = CARTESIAN_POINT ( 'NONE',  ( 0.000000000000000000, 0.000000000000000000, 0.000000000000000000 ) ) ;
#24670 = CARTESIAN_POINT ( 'NONE',  ( -0.05118110236220472370, 0.000000000000000000, 0.000000000000000000 ) ) ;
#24671 = CARTESIAN_POINT ( 'NONE',  ( -6.750021727583836750E-17, -0.5511811023622047445, 0.2637795275590551491 ) ) ;
#24672 = EDGE_CURVE ( 'NONE', #15934, #7615, #18204, .T. ) ;
#24673 = CARTESIAN_POINT ( 'NONE',  ( -0.1447526197146041249, -0.3977045540727763839, 0.1377952755905511861 ) ) ;
#24674 = CARTESIAN_POINT ( 'NONE',  ( 0.5314960629921260393, 0.03478633594540018331, 1.747047244094488194 ) ) ;
#24675 = DIRECTION ( 'NONE',  ( 0.000000000000000000, 0.000000000000000000, -1.000000000000000000 ) ) ;
#24676 = CARTESIAN_POINT ( 'NONE',  ( 0.4856708409200646281, 0.1649135259617043880, 1.766732283464566899 ) ) ;
#24677 = VERTEX_POINT ( 'NONE', #1269 ) ;
#24678 = CARTESIAN_POINT ( 'NONE',  ( -0.09842519685039370636, 0.07874015748031495954, -0.04546065111729338803 ) ) ;
#24679 = VERTEX_POINT ( 'NONE', #27401 ) ;
#24680 = CARTESIAN_POINT ( 'NONE',  ( 0.6711032387266713251, -0.1523958994812761869, 0.3401574803149606252 ) ) ;
#24681 = ( CONVERSION_BASED_UNIT ( 'INCH', #9419 ) LENGTH_UNIT ( ) NAMED_UNIT ( #21899 ) ) ;
#24682 = CARTESIAN_POINT ( 'NONE',  ( -0.4417361510194065533, 0.05819755867303653962, -1.934055118110236338 ) ) ;
#24683 = DIRECTION ( 'NONE',  ( 1.000000000000000000, 0.000000000000000000, 0.000000000000000000 ) ) ;
#24684 = ORIENTED_EDGE ( 'NONE', *, *, #22320, .T. ) ;
#24685 = VERTEX_POINT ( 'NONE', #24696 ) ;
#24686 = CARTESIAN_POINT ( 'NONE',  ( -0.03220957031754000111, 0.4921259842519685179, -1.569881889763779625 ) ) ;
#24687 = CIRCLE ( 'NONE', #16140, 0.02755905511811020808 ) ;
#24688 = VERTEX_POINT ( 'NONE', #1395 ) ;
#24689 = CARTESIAN_POINT ( 'NONE',  ( 0.2442565704126313797, -0.4954197419817796266, 0.9399606299212598381 ) ) ;
#24690 = ORIENTED_EDGE ( 'NONE', *, *, #20054, .T. ) ;
#24691 = CARTESIAN_POINT ( 'NONE',  ( 0.1189624676717049440, -0.3253923344978161825, 0.1377952755905510474 ) ) ;
#24692 = ITEM_DEFINED_TRANSFORMATION ( 'NONE', 'NONE', #22853,  #11588 ) ;
#24693 = DIRECTION ( 'NONE',  ( -0.000000000000000000, 1.000000000000000000, -0.000000000000000000 ) ) ;
#24694 = DIRECTION ( 'NONE',  ( -0.000000000000000000, 1.000000000000000000, -0.000000000000000000 ) ) ;
#24695 = CARTESIAN_POINT ( 'NONE',  ( 0.000000000000000000, 0.000000000000000000, 0.6299212598425196763 ) ) ;
#24696 = CARTESIAN_POINT ( 'NONE',  ( -0.4980314960629921295, 0.000000000000000000, -0.2755905511811023723 ) ) ;
#24697 = CARTESIAN_POINT ( 'NONE',  ( 0.6299212598425196763, 0.000000000000000000, 0.000000000000000000 ) ) ;
#24698 = EDGE_CURVE ( 'NONE', #17997, #1348, #3047, .T. ) ;
#24699 = SPHERICAL_SURFACE ( 'NONE', #24504, 0.07677362204724409722 ) ;
#24700 = EDGE_CURVE ( 'NONE', #26847, #18994, #7126, .T. ) ;
#24701 = AXIS2_PLACEMENT_3D ( 'NONE', #4255, #10886, #6936 ) ;
#24702 = ORIENTED_EDGE ( 'NONE', *, *, #24578, .T. ) ;
#24703 = SHAPE_REPRESENTATION ( 'Front Bearing Cover', ( #11588 ), #10253 ) ;
#24704 = CARTESIAN_POINT ( 'NONE',  ( -0.5379714048901780288, 0.000000000000000000, -0.2342519685039370358 ) ) ;
#24705 = CARTESIAN_POINT ( 'NONE',  ( -0.6463085202143212804, -0.03588704011884780165, 0.2358541165544890683 ) ) ;
#24706 = AXIS2_PLACEMENT_3D ( 'NONE', #12812, #6329, #19600 ) ;
#24707 = CARTESIAN_POINT ( 'NONE',  ( 0.2262947209296605477, -0.4714317853956138671, 0.3331434174482444943 ) ) ;
#24708 = CARTESIAN_POINT ( 'NONE',  ( -0.2223167940359789541, 0.2657206863494903093, 0.1276989850623086176 ) ) ;
#24709 = PRODUCT_DEFINITION_SHAPE ( 'NONE', 'NONE',  #27912 ) ;
#24710 = CARTESIAN_POINT ( 'NONE',  ( -0.4783464566929133688, -0.4724409448818898127, 0.8182917201112815953 ) ) ;
#24711 = ORIENTED_EDGE ( 'NONE', *, *, #26703, .F. ) ;
#24712 = DIRECTION ( 'NONE',  ( 1.000000000000000000, 0.000000000000000000, 0.000000000000000000 ) ) ;
#24713 = AXIS2_PLACEMENT_3D ( 'NONE', #6954, #17801, #22331 ) ;
#24714 = ORIENTED_EDGE ( 'NONE', *, *, #16537, .F. ) ;
#24715 = B_SPLINE_CURVE_WITH_KNOTS ( 'NONE', 3,
 ( #19341, #21334, #27555, #8196, #25424, #14726 ),
 .UNSPECIFIED., .F., .F.,
 ( 4, 2, 4 ),
 ( 0.2376120521391529850, 0.2390783382518550104, 0.2405446243645580073 ),
 .UNSPECIFIED. ) ;
#24716 = PLANE ( 'NONE',  #17462 ) ;
#24717 = EDGE_CURVE ( 'NONE', #19119, #2155, #244, .T. ) ;
#24718 = VERTEX_POINT ( 'NONE', #25272 ) ;
#24719 = B_SPLINE_CURVE_WITH_KNOTS ( 'NONE', 3,
 ( #23143, #10544, #12539, #21154, #1798, #19025 ),
 .UNSPECIFIED., .F., .F.,
 ( 4, 2, 4 ),
 ( 0.2376120521390029938, 0.2390783382518560096, 0.2405446243647090254 ),
 .UNSPECIFIED. ) ;
#24720 = CARTESIAN_POINT ( 'NONE',  ( -0.3220512119205936608, 0.3834984712787528061, 0.09684793308443542803 ) ) ;
#24721 = DIRECTION ( 'NONE',  ( -0.000000000000000000, -1.000000000000000000, -0.000000000000000000 ) ) ;
#24722 = CARTESIAN_POINT ( 'NONE',  ( -0.01288382760289888060, 0.1968503937007873850, -3.646653543307086576 ) ) ;
#24723 = ORIENTED_EDGE ( 'NONE', *, *, #17291, .T. ) ;
#24724 = CARTESIAN_POINT ( 'NONE',  ( -0.3411065095061439068, 0.06065137456822528722, 0.1478915661262500403 ) ) ;
#24725 = CARTESIAN_POINT ( 'NONE',  ( -0.07874015748031495954, 0.1968503937007874127, -3.364501312335958172 ) ) ;
#24726 = EDGE_LOOP ( 'NONE', ( #2157, #14322 ) ) ;
#24727 = CONICAL_SURFACE ( 'NONE', #14848, 0.4724409448465559103, 0.7853981642948979491 ) ;
#24728 = CARTESIAN_POINT ( 'NONE',  ( -0.2118615749922956593, -0.5840192333899354438, 0.09685039370078740717 ) ) ;
#24729 = CIRCLE ( 'NONE', #20218, 0.5007874015748031704 ) ;
#24730 = VECTOR ( 'NONE', #25486, 39.37007874015748143 ) ;
#24731 = FACE_OUTER_BOUND ( 'NONE', #108, .T. ) ;
#24732 = CARTESIAN_POINT ( 'NONE',  ( 0.5309636003393858328, 0.6300167932626280498, -0.5388714850268924161 ) ) ;
#24733 = DIRECTION ( 'NONE',  ( 0.000000000000000000, 0.000000000000000000, -1.000000000000000000 ) ) ;
#24734 = DIRECTION ( 'NONE',  ( 0.000000000000000000, 0.000000000000000000, -1.000000000000000000 ) ) ;
#24735 = VERTEX_POINT ( 'NONE', #25834 ) ;
#24736 = CIRCLE ( 'NONE', #4470, 0.6751968503937006982 ) ;
#24737 = CARTESIAN_POINT ( 'NONE',  ( 0.2521176338356569957, 0.2211428102655756955, 1.973425196850393970 ) ) ;
#24738 = CARTESIAN_POINT ( 'NONE',  ( 0.4921259842519685179, 0.03220957031754003580, -1.550196850393700920 ) ) ;
#24739 = ADVANCED_FACE ( 'NONE', ( #4362, #8187 ), #23459, .T. ) ;
#24740 = CARTESIAN_POINT ( 'NONE',  ( -0.3713448905834433322, 0.06600512665679449109, 0.07637795275590551769 ) ) ;
#24741 = CARTESIAN_POINT ( 'NONE',  ( 0.3642352168757561071, 0.4152525734086270348, 0.9202755905511811330 ) ) ;
#24742 = DIRECTION ( 'NONE',  ( 1.000000000000000000, 0.000000000000000000, 0.000000000000000000 ) ) ;
#24743 = CARTESIAN_POINT ( 'NONE',  ( 0.000000000000000000, 0.000000000000000000, -3.149606299191693548 ) ) ;
#24744 = ORIENTED_EDGE ( 'NONE', *, *, #22214, .T. ) ;
#24745 = CARTESIAN_POINT ( 'NONE',  ( -0.01928643301569672036, 0.07978627494126659669, -0.4680802598521938696 ) ) ;
#24746 = VECTOR ( 'NONE', #10818, 39.37007874015748143 ) ;
#24747 = CARTESIAN_POINT ( 'NONE',  ( 0.4423390553432540173, 0.2180862235769270852, -1.569881889763779625 ) ) ;
#24748 = CONICAL_SURFACE ( 'NONE', #26534, 0.4092416079569000109, 0.7340599135827593491 ) ;
#24749 = CIRCLE ( 'NONE', #15317, 0.6881889763779527325 ) ;
#24750 = CARTESIAN_POINT ( 'NONE',  ( 0.03532354024591712049, -0.8267716535433071723, 0.000000000000000000 ) ) ;
#24751 = DIRECTION ( 'NONE',  ( 1.000000000000000000, 0.000000000000000000, 0.000000000000000000 ) ) ;
#24752 = CARTESIAN_POINT ( 'NONE',  ( 0.6102362204724409711, 0.000000000000000000, 0.2362204724409449064 ) ) ;
#24753 = CARTESIAN_POINT ( 'NONE',  ( 0.000000000000000000, 0.000000000000000000, 0.1992125984251968684 ) ) ;
#24754 = EDGE_CURVE ( 'NONE', #21183, #19404, #19931, .T. ) ;
#24755 = EDGE_LOOP ( 'NONE', ( #17678, #20280 ) ) ;
#24756 = DIRECTION ( 'NONE',  ( 1.000000000000000000, 0.000000000000000000, 0.000000000000000000 ) ) ;
#24757 = FACE_OUTER_BOUND ( 'NONE', #4150, .T. ) ;
#24758 = ORIENTED_EDGE ( 'NONE', *, *, #2752, .T. ) ;
#24759 = CARTESIAN_POINT ( 'NONE',  ( -0.2669897767696617907, 0.2341075107471362882, 1.953740157480315487 ) ) ;
#24760 = VERTEX_POINT ( 'NONE', #27545 ) ;
#24761 = CARTESIAN_POINT ( 'NONE',  ( -0.1173917140416368271, -0.4382752542996092293, -1.934055118110236338 ) ) ;
#24762 = CYLINDRICAL_SURFACE ( 'NONE', #14356, 0.5118110236220472231 ) ;
#24763 = DIRECTION ( 'NONE',  ( 0.000000000000000000, -1.000000000000000000, 0.000000000000000000 ) ) ;
#24764 = CARTESIAN_POINT ( 'NONE',  ( 0.1522836969735573143, -0.1970374587079578854, 0.4531137400369409374 ) ) ;
#24765 = CARTESIAN_POINT ( 'NONE',  ( 0.2303471512294322787, -0.4798602677570401598, 0.1322834645669291320 ) ) ;
#24766 = DIRECTION ( 'NONE',  ( 0.000000000000000000, 0.000000000000000000, 1.000000000000000000 ) ) ;
#24767 = CARTESIAN_POINT ( 'NONE',  ( 0.000000000000000000, 0.000000000000000000, 0.3543307086614173040 ) ) ;
#24768 = VERTEX_POINT ( 'NONE', #27821 ) ;
#24769 = CARTESIAN_POINT ( 'NONE',  ( 0.3872945158171015589, 4.742989891227373650E-17, -0.2342519685039370358 ) ) ;
#24770 = AXIS2_PLACEMENT_3D ( 'NONE', #26790, #14528, #3041 ) ;
#24771 = DIRECTION ( 'NONE',  ( 1.000000000000000000, 0.000000000000000000, 0.000000000000000000 ) ) ;
#24772 = ORIENTED_EDGE ( 'NONE', *, *, #3062, .F. ) ;
#24773 = CARTESIAN_POINT ( 'NONE',  ( -0.2993674444872274076, -0.2296683860596782090, -3.100567304031764060 ) ) ;
#24774 = AXIS2_PLACEMENT_3D ( 'NONE', #10464, #10604, #23898 ) ;
#24775 = CARTESIAN_POINT ( 'NONE',  ( 0.2362017869179295071, -0.2693781226336162127, -3.115157480314961091 ) ) ;
#24776 = APPLICATION_CONTEXT ( 'automotive_design' ) ;
#24777 = EDGE_CURVE ( 'NONE', #23387, #12348, #7478, .T. ) ;
#24778 = VERTEX_POINT ( 'NONE', #1680 ) ;
#24779 = CARTESIAN_POINT ( 'NONE',  ( -0.3599896729929454864, 0.2761764805255169652, -1.934055118110236338 ) ) ;
#24780 = ADVANCED_FACE ( 'NONE', ( #4228 ), #12562, .T. ) ;
#24781 = B_SPLINE_CURVE_WITH_KNOTS ( 'NONE', 3,
 ( #25876, #4404, #19512, #6666 ),
 .UNSPECIFIED., .F., .F.,
 ( 4, 4 ),
 ( 0.7157687286427140139, 0.7172350147555668354 ),
 .UNSPECIFIED. ) ;
#24782 = APPLICATION_PROTOCOL_DEFINITION ( 'draft international standard', 'automotive_design', 1998, #9969 ) ;
#24783 = CARTESIAN_POINT ( 'NONE',  ( 0.5604501195232224342, 0.4479362078551570869, 0.1601585119463994344 ) ) ;
#24784 = CARTESIAN_POINT ( 'NONE',  ( 0.000000000000000000, 0.000000000000000000, 0.2362204724409449064 ) ) ;
#24785 = CARTESIAN_POINT ( 'NONE',  ( 0.03349795313264414959, -0.5118110236220472231, 1.747047244094488194 ) ) ;
#24786 = ORIENTED_EDGE ( 'NONE', *, *, #15046, .T. ) ;
#24787 = AXIS2_PLACEMENT_3D ( 'NONE', #772, #1057, #24620 ) ;
#24788 = ORIENTED_EDGE ( 'NONE', *, *, #22931, .T. ) ;
#24789 = DIMENSIONAL_EXPONENTS ( 1.000000000000000000, 0.000000000000000000, 0.000000000000000000, 0.000000000000000000, 0.000000000000000000, 0.000000000000000000, 0.000000000000000000 ) ;
#24790 = CIRCLE ( 'NONE', #27065, 0.3771653543307086909 ) ;
#24791 = CARTESIAN_POINT ( 'NONE',  ( 0.04928467685643810742, 0.3740848232703744003, -3.100567304031763172 ) ) ;
#24792 = DIRECTION ( 'NONE',  ( 0.000000000000000000, 0.000000000000000000, -1.000000000000000000 ) ) ;
#24793 = CARTESIAN_POINT ( 'NONE',  ( 0.000000000000000000, 0.000000000000000000, 0.4062992125984251635 ) ) ;
#24794 = EDGE_CURVE ( 'NONE', #16332, #8070, #12879, .T. ) ;
#24795 = ORIENTED_EDGE ( 'NONE', *, *, #4503, .T. ) ;
#24796 = CARTESIAN_POINT ( 'NONE',  ( -0.4284035790182393888, -0.5294929124318047409, -0.4312010047435373972 ) ) ;
#24797 = FACE_OUTER_BOUND ( 'NONE', #14333, .T. ) ;
#24798 = ORIENTED_EDGE ( 'NONE', *, *, #12284, .T. ) ;
#24799 = CARTESIAN_POINT ( 'NONE',  ( 0.2712027394948692827, 0.3535065162672724748, -1.934055118110236338 ) ) ;
#24800 = ORIENTED_EDGE ( 'NONE', *, *, #3260, .T. ) ;
#24801 = ORIENTED_EDGE ( 'NONE', *, *, #2752, .F. ) ;
#24802 = DIRECTION ( 'NONE',  ( 0.000000000000000000, 1.000000000000000000, 0.000000000000000000 ) ) ;
#24803 = DIRECTION ( 'NONE',  ( -1.000000000000000000, 0.000000000000000000, 0.000000000000000000 ) ) ;
#24804 = DIRECTION ( 'NONE',  ( 0.000000000000000000, 1.000000000000000000, 0.000000000000000000 ) ) ;
#24805 = DIRECTION ( 'NONE',  ( 0.000000000000000000, 0.000000000000000000, 1.000000000000000000 ) ) ;
#24806 = DIRECTION ( 'NONE',  ( 0.000000000000000000, 0.000000000000000000, -1.000000000000000000 ) ) ;
#24807 = DIRECTION ( 'NONE',  ( 0.000000000000000000, 1.000000000000000000, 0.000000000000000000 ) ) ;
#24808 = FACE_OUTER_BOUND ( 'NONE', #18466, .T. ) ;
#24809 = CIRCLE ( 'NONE', #12639, 0.8163976377952757435 ) ;
#24810 = CONICAL_SURFACE ( 'NONE', #3143, 0.4626586504047134341, 0.3230892413134545116 ) ;
#24811 = CARTESIAN_POINT ( 'NONE',  ( 0.000000000000000000, -5.457511811023621697E-17, -0.1696422624804970747 ) ) ;
#24812 = B_SPLINE_CURVE_WITH_KNOTS ( 'NONE', 3,
 ( #5000, #26609, #15885, #24627 ),
 .UNSPECIFIED., .F., .F.,
 ( 4, 4 ),
 ( 0.3015484798814578316, 0.3030532441042709801 ),
 .UNSPECIFIED. ) ;
#24813 = CARTESIAN_POINT ( 'NONE',  ( 0.000000000000000000, 0.000000000000000000, 0.2362204724409449064 ) ) ;
#24814 = CARTESIAN_POINT ( 'NONE',  ( 0.5383572925355708527, -0.3100567972184350429, 0.2574803149606298969 ) ) ;
#24815 = VERTEX_POINT ( 'NONE', #21179 ) ;
#24816 = DIRECTION ( 'NONE',  ( 0.000000000000000000, 0.000000000000000000, 1.000000000000000000 ) ) ;
#24817 = CARTESIAN_POINT ( 'NONE',  ( -0.5378064472801062923, -0.3110113600220464902, 0.09684874924366436433 ) ) ;
#24818 = MECHANICAL_DESIGN_GEOMETRIC_PRESENTATION_REPRESENTATION (  '', ( #22119 ), #6791 ) ;
#24819 = CARTESIAN_POINT ( 'NONE',  ( 3.387491338582676985E-16, -0.6299212598425196763, -0.5915354330708662012 ) ) ;
#24820 = DIRECTION ( 'NONE',  ( 1.000000000000000000, 0.000000000000000000, 0.000000000000000000 ) ) ;
#24821 = EDGE_LOOP ( 'NONE', ( #5480, #2879, #23213, #11229, #21892 ) ) ;
#24822 = FACE_OUTER_BOUND ( 'NONE', #25953, .T. ) ;
#24823 = CARTESIAN_POINT ( 'NONE',  ( -0.4777261797697572310, -0.2355331214654124150, 1.747047244094488194 ) ) ;
#24824 = DIRECTION ( 'NONE',  ( 0.000000000000000000, 0.000000000000000000, -1.000000000000000000 ) ) ;
#24825 = ADVANCED_BREP_SHAPE_REPRESENTATION ( 'Barrel Cam', ( #3396, #11588 ), #18804 ) ;
#24826 = CARTESIAN_POINT ( 'NONE',  ( -0.4954415918530846175, -0.1327036767659680039, 1.766732283464566899 ) ) ;
#24827 = VERTEX_POINT ( 'NONE', #8053 ) ;
#24828 = ORIENTED_EDGE ( 'NONE', *, *, #11571, .T. ) ;
#24829 = CARTESIAN_POINT ( 'NONE',  ( 0.2255758929760254272, -0.6217623271433985188, 0.1926811207689738403 ) ) ;
#24830 = ADVANCED_FACE ( 'NONE', ( #25414, #15119 ), #23728, .T. ) ;
#24831 = CARTESIAN_POINT ( 'NONE',  ( 0.3100894960467185379, -0.1796141127317343322, 0.09506557083533939689 ) ) ;
#24832 = ORIENTED_EDGE ( 'NONE', *, *, #5174, .F. ) ;
#24833 = EDGE_LOOP ( 'NONE', ( #8176, #12726, #10988, #18461, #2084 ) ) ;
#24834 = AXIS2_PLACEMENT_3D ( 'NONE', #18003, #24252, #13798 ) ;
#24835 = CARTESIAN_POINT ( 'NONE',  ( 0.3707612262533033776, -0.3252100150720387273, -1.569881889763779625 ) ) ;
#24836 = PRODUCT_RELATED_PRODUCT_CATEGORY ( 'part', '', ( #21073 ) ) ;
#24837 = VERTEX_POINT ( 'NONE', #4088 ) ;
#24838 = ORIENTED_EDGE ( 'NONE', *, *, #18061, .F. ) ;
#24839 = VERTEX_POINT ( 'NONE', #5934 ) ;
#24840 = EDGE_CURVE ( 'NONE', #4007, #17345, #25459, .T. ) ;
#24841 = ORIENTED_EDGE ( 'NONE', *, *, #20172, .T. ) ;
#24842 = AXIS2_PLACEMENT_3D ( 'NONE', #4199, #23292, #25109 ) ;
#24843 = CONTEXT_DEPENDENT_SHAPE_REPRESENTATION ( #15960, #8911 ) ;
#24844 = ADVANCED_FACE ( 'NONE', ( #25697 ), #1820, .F. ) ;
#24845 = DIRECTION ( 'NONE',  ( 0.000000000000000000, 1.000000000000000000, 0.000000000000000000 ) ) ;
#24846 = CARTESIAN_POINT ( 'NONE',  ( 0.000000000000000000, 0.000000000000000000, 0.1377952755905511861 ) ) ;
#24847 = PLANE ( 'NONE',  #11825 ) ;
#24848 = CARTESIAN_POINT ( 'NONE',  ( 0.000000000000000000, 0.000000000000000000, 0.07637795275590551769 ) ) ;
#24849 = CARTESIAN_POINT ( 'NONE',  ( 0.5096726623840048820, -0.1170085733297153430, 0.3331434174570839235 ) ) ;
#24850 = CARTESIAN_POINT ( 'NONE',  ( -0.2521176338356424518, 0.2211428102655600414, 1.953740157480315043 ) ) ;
#24851 = UNCERTAINTY_MEASURE_WITH_UNIT (LENGTH_MEASURE( 1.000000000000000082E-05 ), #26069, 'distance_accuracy_value', 'NONE') ;
#24852 = CARTESIAN_POINT ( 'NONE',  ( -0.1771653543307086520, 1.241643108977391477E-17, 0.1476377952755905387 ) ) ;
#24853 = CARTESIAN_POINT ( 'NONE',  ( 0.4062254136079394562, -0.2349793847444826833, 0.07637630773773071424 ) ) ;
#24854 = AXIS2_PLACEMENT_3D ( 'NONE', #26745, #18100, #9222 ) ;
#24855 = CARTESIAN_POINT ( 'NONE',  ( -0.09842519685039370636, 0.5905905511811023745, -3.548228346456693050 ) ) ;
#24856 = DIRECTION ( 'NONE',  ( 0.8660254037844387076, 0.4999999999999998890, -0.000000000000000000 ) ) ;
#24857 = DIRECTION ( 'NONE',  ( -1.000000000000000000, 1.224646799147353454E-16, 0.000000000000000000 ) ) ;
#24858 = VECTOR ( 'NONE', #11707, 39.37007874015748143 ) ;
#24859 = ORIENTED_EDGE ( 'NONE', *, *, #9312, .T. ) ;
#24860 = DIRECTION ( 'NONE',  ( 0.000000000000000000, 0.000000000000000000, -1.000000000000000000 ) ) ;
#24861 = ORIENTED_EDGE ( 'NONE', *, *, #23798, .F. ) ;
#24862 = FACE_OUTER_BOUND ( 'NONE', #2619, .T. ) ;
#24863 = ORIENTED_EDGE ( 'NONE', *, *, #2871, .T. ) ;
#24864 = DIRECTION ( 'NONE',  ( 0.000000000000000000, 1.000000000000000000, 0.000000000000000000 ) ) ;
#24865 = PLANE ( 'NONE',  #11651 ) ;
#24866 = CARTESIAN_POINT ( 'NONE',  ( -0.06048688226689268727, 0.1968503937007873850, -3.626935712454880001 ) ) ;
#24867 = EDGE_LOOP ( 'NONE', ( #24192, #18315, #1524, #18467 ) ) ;
#24868 = EDGE_CURVE ( 'NONE', #26728, #13078, #1556, .T. ) ;
#24869 = DIRECTION ( 'NONE',  ( 0.000000000000000000, 0.000000000000000000, 1.000000000000000000 ) ) ;
#24870 = ORIENTED_EDGE ( 'NONE', *, *, #25443, .T. ) ;
#24871 = ADVANCED_FACE ( 'NONE', ( #5038 ), #11468, .T. ) ;
#24872 = CARTESIAN_POINT ( 'NONE',  ( -0.3002886982018051487, -0.1727973894384558229, 0.1377952755905512416 ) ) ;
#24873 = DIRECTION ( 'NONE',  ( -1.000000000000000000, 0.000000000000000000, -0.000000000000000000 ) ) ;
#24874 = AXIS2_PLACEMENT_3D ( 'NONE', #1422, #14744, #12155 ) ;
#24875 = VECTOR ( 'NONE', #2712, 39.37007874015748854 ) ;
#24876 = DIRECTION ( 'NONE',  ( 0.000000000000000000, 0.000000000000000000, 1.000000000000000000 ) ) ;
#24877 = ORIENTED_EDGE ( 'NONE', *, *, #13941, .T. ) ;
#24878 = CARTESIAN_POINT ( 'NONE',  ( 0.000000000000000000, 0.07874015748662489822, 0.000000000000000000 ) ) ;
#24879 = EDGE_LOOP ( 'NONE', ( #10167, #14231, #10972, #1432 ) ) ;
#24880 = CARTESIAN_POINT ( 'NONE',  ( -0.3324885138898239778, 0.04380447413658877104, 1.973425196850393970 ) ) ;
#24881 = CARTESIAN_POINT ( 'NONE',  ( -0.4930758245789425009, 0.08754571829529331217, 0.2574803149606298969 ) ) ;
#24882 = CARTESIAN_POINT ( 'NONE',  ( -0.4954415918535808872, -0.1327036767636090853, -1.550196850393700920 ) ) ;
#24883 = EDGE_CURVE ( 'NONE', #21302, #16931, #13274, .T. ) ;
#24884 = CARTESIAN_POINT ( 'NONE',  ( 0.1442704874421230632, 0.5368353335967094297, 0.9202755905511812440 ) ) ;
#24885 = CARTESIAN_POINT ( 'NONE',  ( 0.2442565704126255510, -0.4954197419817655823, 0.9202755905511811330 ) ) ;
#24886 = CARTESIAN_POINT ( 'NONE',  ( 0.000000000000000000, 0.000000000000000000, 0.2637795275590551491 ) ) ;
#24887 = ORIENTED_EDGE ( 'NONE', *, *, #10585, .T. ) ;
#24888 = PRODUCT_DEFINITION_SHAPE ( 'NONE', 'NONE',  #24464 ) ;
#24889 = CARTESIAN_POINT ( 'NONE',  ( -0.05938807134538628962, 0.05663358325667527948, -0.4684893292439903378 ) ) ;
#24890 = CYLINDRICAL_SURFACE ( 'NONE', #27500, 0.3937007873768824662 ) ;
#24891 = FILL_AREA_STYLE ('',( #7812 ) ) ;
#24892 = AXIS2_PLACEMENT_3D ( 'NONE', #3382, #14155, #27425 ) ;
#24893 = CARTESIAN_POINT ( 'NONE',  ( 0.4282978893168862267, 0.1305933181008684940, 0.2362204724409449896 ) ) ;
#24894 = CARTESIAN_POINT ( 'NONE',  ( -0.4763779527559054983, 0.000000000000000000, -0.01377952755905511792 ) ) ;
#24895 = CARTESIAN_POINT ( 'NONE',  ( -0.09842519685039370636, 2.800920866141732248E-17, 0.09092130223458683158 ) ) ;
#24896 = VERTEX_POINT ( 'NONE', #11267 ) ;
#24897 = DIRECTION ( 'NONE',  ( 0.000000000000000000, 0.000000000000000000, 1.000000000000000000 ) ) ;
#24898 = FACE_OUTER_BOUND ( 'NONE', #7211, .T. ) ;
#24899 = DIRECTION ( 'NONE',  ( 1.000000000000000000, 7.017815000000000124E-18, 0.000000000000000000 ) ) ;
#24900 = EDGE_CURVE ( 'NONE', #4805, #9518, #17356, .T. ) ;
#24901 = ORIENTED_EDGE ( 'NONE', *, *, #11136, .T. ) ;
#24902 = CARTESIAN_POINT ( 'NONE',  ( 0.3070866141732283561, 0.000000000000000000, 0.2637795275590551491 ) ) ;
#24903 = ORIENTED_EDGE ( 'NONE', *, *, #26454, .T. ) ;
#24904 = CARTESIAN_POINT ( 'NONE',  ( -0.4308867145613631822, -0.2480839813575886066, 0.1615162260909178693 ) ) ;
#24905 = CARTESIAN_POINT ( 'NONE',  ( 0.5699748819085377338, -0.3282885190152939336, 0.1461456498327310671 ) ) ;
#24906 = DIRECTION ( 'NONE',  ( 0.000000000000000000, 1.000000000000000000, 0.000000000000000000 ) ) ;
#24907 = CARTESIAN_POINT ( 'NONE',  ( 0.3713448905834433322, 0.06600512665679410251, 0.07637795275590551769 ) ) ;
#24908 = FACE_OUTER_BOUND ( 'NONE', #2961, .T. ) ;
#24909 = ORIENTED_EDGE ( 'NONE', *, *, #7871, .T. ) ;
#24910 = CARTESIAN_POINT ( 'NONE',  ( 0.1285103288269283661, -0.3545966721392122545, 0.07637795275590551769 ) ) ;
#24911 = AXIS2_PLACEMENT_3D ( 'NONE', #8986, #2493, #23972 ) ;
#24912 = LINE ( 'NONE', #20399, #12098 ) ;
#24913 = AXIS2_PLACEMENT_3D ( 'NONE', #11569, #569, #5211 ) ;
#24914 = DIRECTION ( 'NONE',  ( 0.000000000000000000, -1.000000000000000000, 0.000000000000000000 ) ) ;
#24915 = VERTEX_POINT ( 'NONE', #2640 ) ;
#24916 = CARTESIAN_POINT ( 'NONE',  ( -0.07217847769028858107, -4.927204724409449161E-18, 0.000000000000000000 ) ) ;
#24917 = ADVANCED_FACE ( 'NONE', ( #10998, #22139 ), #7166, .T. ) ;
#24918 = PRODUCT_DEFINITION_CONTEXT ( 'detailed design', #5484, 'design' ) ;
#24919 = VERTEX_POINT ( 'NONE', #13109 ) ;
#24920 = CARTESIAN_POINT ( 'NONE',  ( 0.02909913904661943010, -0.4446020952038907681, -1.934055118110236338 ) ) ;
#24921 = VERTEX_POINT ( 'NONE', #21738 ) ;
#24922 = EDGE_LOOP ( 'NONE', ( #17513, #20638, #3897, #5774 ) ) ;
#24923 = CARTESIAN_POINT ( 'NONE',  ( -0.3338887748335570560, -0.9590537645700274449, -0.8833427619775512385 ) ) ;
#24924 = DIRECTION ( 'NONE',  ( 1.000000000000000000, 7.017815000000000124E-18, 0.000000000000000000 ) ) ;
#24925 = CARTESIAN_POINT ( 'NONE',  ( 0.3412792617076849666, 0.05967164814832574826, 0.1478915661242290458 ) ) ;
#24926 = CIRCLE ( 'NONE', #17703, 0.6881889763779527325 ) ;
#24927 = ORIENTED_EDGE ( 'NONE', *, *, #23168, .F. ) ;
#24928 = VECTOR ( 'NONE', #1268, 39.37007874015748143 ) ;
#24929 = DIRECTION ( 'NONE',  ( 1.000000000000000000, 0.000000000000000000, 0.000000000000000000 ) ) ;
#24930 = CIRCLE ( 'NONE', #10968, 0.5511811023622047445 ) ;
#24931 = CARTESIAN_POINT ( 'NONE',  ( -0.08294224740493445769, -0.2381676936971315051, -0.2581876938019334600 ) ) ;
#24932 = EDGE_CURVE ( 'NONE', #21621, #10030, #8137, .T. ) ;
#24933 = EDGE_LOOP ( 'NONE', ( #13430, #4494, #26526, #17444 ) ) ;
#24934 = AXIS2_PLACEMENT_3D ( 'NONE', #14165, #18364, #23631 ) ;
#24935 = DIRECTION ( 'NONE',  ( -1.000000000000000000, 1.224646799147353454E-16, 0.000000000000000000 ) ) ;
#24936 = CARTESIAN_POINT ( 'NONE',  ( 0.03532354024591720376, -0.8267716535433071723, 0.000000000000000000 ) ) ;
#24937 = VERTEX_POINT ( 'NONE', #26500 ) ;
#24938 = CARTESIAN_POINT ( 'NONE',  ( 0.3349573549949902418, -0.2938049579018460755, -1.934055118110236338 ) ) ;
#24939 = ORIENTED_EDGE ( 'NONE', *, *, #25653, .T. ) ;
#24940 = EDGE_LOOP ( 'NONE', ( #1022, #27456, #20518, #20289 ) ) ;
#24941 = DIRECTION ( 'NONE',  ( -0.4999999999999995004, -0.8660254037844390407, 0.000000000000000000 ) ) ;
#24942 = DIRECTION ( 'NONE',  ( -0.9009688679024190350, -0.4338837391175581759, 0.000000000000000000 ) ) ;
#24943 = CARTESIAN_POINT ( 'NONE',  ( 0.3213305936751379432, -0.1584254766472190656, -3.115157480314960647 ) ) ;
#24944 = DIRECTION ( 'NONE',  ( 0.9930684569549264040, -0.05876869872891801738, -0.1017903720931950112 ) ) ;
#24945 = CARTESIAN_POINT ( 'NONE',  ( 0.6397637795275591399, 0.000000000000000000, 0.000000000000000000 ) ) ;
#24946 = DIRECTION ( 'NONE',  ( 0.000000000000000000, 0.000000000000000000, -1.000000000000000000 ) ) ;
#24947 = PRODUCT ( 'Output Shaft', 'Output Shaft', '', ( #9108 ) ) ;
#24948 = CIRCLE ( 'NONE', #6014, 0.1299232283464567261 ) ;
#24949 = ADVANCED_FACE ( 'NONE', ( #11537 ), #5614, .T. ) ;
#24950 = CARTESIAN_POINT ( 'NONE',  ( 0.000000000000000000, 0.000000000000000000, -4.291338582656260670 ) ) ;
#24951 = VECTOR ( 'NONE', #19810, 39.37007874015748143 ) ;
#24952 = LINE ( 'NONE', #16069, #13434 ) ;
#24953 = CARTESIAN_POINT ( 'NONE',  ( -0.3661417322834645272, -0.4724409448818898127, -0.7100240035758484947 ) ) ;
#24954 = CONICAL_SURFACE ( 'NONE', #12779, 0.4526932812344527379, 0.1178097243749990780 ) ;
#24955 = ORIENTED_EDGE ( 'NONE', *, *, #9281, .F. ) ;
#24956 = CARTESIAN_POINT ( 'NONE',  ( -0.5383572925356228112, -0.3100567972183445042, 0.2574803149606298969 ) ) ;
#24957 = TOROIDAL_SURFACE ( 'NONE', #4206, 0.6102362204724409711, 0.1299212598425196763 ) ;
#24958 = B_SPLINE_CURVE_WITH_KNOTS ( 'NONE', 3,
 ( #2023, #21904, #16874, #2535 ),
 .UNSPECIFIED., .F., .F.,
 ( 4, 4 ),
 ( 0.9101643785142677912, 1.000000000000000000 ),
 .UNSPECIFIED. ) ;
#24959 = CARTESIAN_POINT ( 'NONE',  ( 0.000000000000000000, 0.5610236220472440971, -3.341531889763779686E-17 ) ) ;
#24960 = CARTESIAN_POINT ( 'NONE',  ( -0.3268939675028499914, -0.1881330340946393564, 0.07637795275590551769 ) ) ;
#24961 = AXIS2_PLACEMENT_3D ( 'NONE', #958, #9545, #11820 ) ;
#24962 = CARTESIAN_POINT ( 'NONE',  ( 0.000000000000000000, 0.000000000000000000, -1.092739370078740131E-17 ) ) ;
#24963 = CARTESIAN_POINT ( 'NONE',  ( 0.5144970376936013334, 0.1378076643338890239, 1.747047244094488194 ) ) ;
#24964 = CARTESIAN_POINT ( 'NONE',  ( -0.2564944395515788567, -0.4441657790107717552, 1.766732283464566899 ) ) ;
#24965 = ORIENTED_EDGE ( 'NONE', *, *, #25342, .T. ) ;
#24966 = ORIENTED_EDGE ( 'NONE', *, *, #18908, .F. ) ;
#24967 = CARTESIAN_POINT ( 'NONE',  ( -0.2490711204941346568, 0.7655264129003995777, -0.7689379837741201484 ) ) ;
#24968 = ORIENTED_EDGE ( 'NONE', *, *, #24024, .F. ) ;
#24969 = CYLINDRICAL_SURFACE ( 'NONE', #6926, 0.1082677165354330728 ) ;
#24970 = CARTESIAN_POINT ( 'NONE',  ( 0.7872492283035658067, 0.4002685408453414140, 0.1724957412521976319 ) ) ;
#24971 = CARTESIAN_POINT ( 'NONE',  ( -0.1447526197146041249, -0.3977045540727763839, 0.1377952755905511861 ) ) ;
#24972 = EDGE_CURVE ( 'NONE', #20656, #4466, #3777, .T. ) ;
#24973 = DIRECTION ( 'NONE',  ( -1.000000000000000000, 0.000000000000000000, 0.000000000000000000 ) ) ;
#24974 = ORIENTED_EDGE ( 'NONE', *, *, #7954, .T. ) ;
#24975 = EDGE_LOOP ( 'NONE', ( #4363, #21314 ) ) ;
#24976 = CARTESIAN_POINT ( 'NONE',  ( 0.4921259842519685179, 0.03220957031754003580, -1.569881889763779625 ) ) ;
#24977 = ORIENTED_EDGE ( 'NONE', *, *, #3137, .T. ) ;
#24978 = EDGE_LOOP ( 'NONE', ( #22745, #19939, #10302, #20647 ) ) ;
#24979 = ORIENTED_EDGE ( 'NONE', *, *, #17069, .T. ) ;
#24980 = ORIENTED_EDGE ( 'NONE', *, *, #21633, .F. ) ;
#24981 = CONTEXT_DEPENDENT_SHAPE_REPRESENTATION ( #6768, #20202 ) ;
#24982 = DIRECTION ( 'NONE',  ( 0.000000000000000000, 0.000000000000000000, 1.000000000000000000 ) ) ;
#24983 = AXIS2_PLACEMENT_3D ( 'NONE', #9588, #26982, #20196 ) ;
#24984 = DIRECTION ( 'NONE',  ( 0.000000000000000000, 0.000000000000000000, 1.000000000000000000 ) ) ;
#24985 = CARTESIAN_POINT ( 'NONE',  ( 0.4622619257814448712, 0.08092139668561752763, 0.1992125984251968684 ) ) ;
#24986 = CARTESIAN_POINT ( 'NONE',  ( 0.1259842519685039353, 0.000000000000000000, 0.000000000000000000 ) ) ;
#24987 = FACE_OUTER_BOUND ( 'NONE', #21306, .T. ) ;
#24988 = ORIENTED_EDGE ( 'NONE', *, *, #27793, .F. ) ;
#24989 = CARTESIAN_POINT ( 'NONE',  ( 0.1522836969735573143, -0.4909267390297480382, -0.05591742528025173131 ) ) ;
#24990 = DIRECTION ( 'NONE',  ( 0.000000000000000000, 0.000000000000000000, -1.000000000000000000 ) ) ;
#24991 = EDGE_CURVE ( 'NONE', #27369, #7273, #25000, .T. ) ;
#24992 = DIRECTION ( 'NONE',  ( 1.000000000000000000, 0.000000000000000000, 0.000000000000000000 ) ) ;
#24993 = CARTESIAN_POINT ( 'NONE',  ( -0.06001958459474839719, -0.4555658499976154574, -1.928289503579151187 ) ) ;
#24994 = CARTESIAN_POINT ( 'NONE',  ( 0.1606879121749082706, -0.4409237942971039881, 0.1992150590373740204 ) ) ;
#24995 = CARTESIAN_POINT ( 'NONE',  ( -0.1288129352161812291, 0.4793172621399193756, -1.569881889763779848 ) ) ;
#24996 = CARTESIAN_POINT ( 'NONE',  ( -0.4084310843276608982, 0.3265597623319961840, 0.1392975274211175618 ) ) ;
#24997 = CIRCLE ( 'NONE', #24526, 0.4685039370078740717 ) ;
#24998 = VERTEX_POINT ( 'NONE', #13945 ) ;
#24999 = EDGE_CURVE ( 'NONE', #19022, #3726, #24524, .T. ) ;
#25000 = CIRCLE ( 'NONE', #645, 0.02755905511811020808 ) ;
#25001 = VERTEX_POINT ( 'NONE', #14379 ) ;
#25002 = ORIENTED_EDGE ( 'NONE', *, *, #6905, .T. ) ;
#25003 = CARTESIAN_POINT ( 'NONE',  ( -0.1649135259639108730, -0.4856708409191554665, -1.550196850393700920 ) ) ;
#25004 = FACE_OUTER_BOUND ( 'NONE', #27643, .T. ) ;
#25005 = CARTESIAN_POINT ( 'NONE',  ( 0.000000000000000000, 0.1968503937007875237, 0.000000000000000000 ) ) ;
#25006 = ORIENTED_EDGE ( 'NONE', *, *, #19515, .F. ) ;
#25007 = DIRECTION ( 'NONE',  ( -1.000000000000000000, -1.224646799147356165E-16, 0.000000000000000000 ) ) ;
#25008 = VECTOR ( 'NONE', #1832, 39.37007874015748854 ) ;
#25009 = CARTESIAN_POINT ( 'NONE',  ( -0.2979095355689177493, -0.6203660015065670663, 0.3401574803149606252 ) ) ;
#25010 = EDGE_LOOP ( 'NONE', ( #4081, #13232, #19005, #20044, #20457, #275 ) ) ;
#25011 = CARTESIAN_POINT ( 'NONE',  ( 0.5385210225480960844, 0.4284847435812472183, 0.3401574803149606252 ) ) ;
#25012 = CARTESIAN_POINT ( 'NONE',  ( 0.000000000000000000, 0.000000000000000000, 0.1377952755905511861 ) ) ;
#25013 = CARTESIAN_POINT ( 'NONE',  ( 0.6881889763779527325, 0.000000000000000000, 0.3401574803149606252 ) ) ;
#25014 = AXIS2_PLACEMENT_3D ( 'NONE', #5517, #9886, #1279 ) ;
#25015 = CARTESIAN_POINT ( 'NONE',  ( 0.1109424284362303254, -0.2012500529900838608, -2.464602332225414408E-17 ) ) ;
#25016 = ORIENTED_EDGE ( 'NONE', *, *, #27371, .F. ) ;
#25017 = CARTESIAN_POINT ( 'NONE',  ( -0.6241612307011117355, 0.1093779649451541158, 0.2481708550935493307 ) ) ;
#25018 = CIRCLE ( 'NONE', #16456, 0.2362204724225640262 ) ;
#25019 = ORIENTED_EDGE ( 'NONE', *, *, #15940, .F. ) ;
#25020 = ORIENTED_EDGE ( 'NONE', *, *, #1983, .T. ) ;
#25021 = B_SPLINE_CURVE_WITH_KNOTS ( 'NONE', 3,
 ( #22077, #6979, #24201, #15339, #16771, #10792 ),
 .UNSPECIFIED., .F., .F.,
 ( 4, 2, 4 ),
 ( 1.162880698919837918, 1.164573402063411978, 1.166266105206986037 ),
 .UNSPECIFIED. ) ;
#25022 = CARTESIAN_POINT ( 'NONE',  ( 0.5085118447796558305, 0.06699507805605002531, -1.550196850393700920 ) ) ;
#25023 = CARTESIAN_POINT ( 'NONE',  ( -0.4407612517155324872, 0.3387265385688508212, 0.9202755905511812440 ) ) ;
#25024 = EDGE_CURVE ( 'NONE', #10256, #15244, #11939, .T. ) ;
#25025 = B_SPLINE_CURVE_WITH_KNOTS ( 'NONE', 3,
 ( #10594, #25860, #6509, #15141, #23752, #13684, #842, #5206 ),
 .UNSPECIFIED., .F., .F.,
 ( 4, 2, 2, 4 ),
 ( 0.5000000000000000000, 0.7500000000000000000, 0.8750000000000000000, 1.000000000000000000 ),
 .UNSPECIFIED. ) ;
#25026 = CARTESIAN_POINT ( 'NONE',  ( -0.1447526197146041249, -0.3977045540727763839, 0.1377952755905511861 ) ) ;
#25027 = CARTESIAN_POINT ( 'NONE',  ( -0.5511811023622047445, 0.000000000000000000, 0.9202755905511811330 ) ) ;
#25028 = CARTESIAN_POINT ( 'NONE',  ( -0.3002886982018052042, -0.1727973894384558229, 0.1478915661221150424 ) ) ;
#25029 = EDGE_CURVE ( 'NONE', #17458, #5345, #9670, .T. ) ;
#25030 = CARTESIAN_POINT ( 'NONE',  ( -0.1189624676717059848, -0.3253923344978159604, 0.1377952755905513249 ) ) ;
#25031 = ORIENTED_EDGE ( 'NONE', *, *, #21603, .T. ) ;
#25032 = DIRECTION ( 'NONE',  ( 0.000000000000000000, 0.000000000000000000, 1.000000000000000000 ) ) ;
#25033 = EDGE_CURVE ( 'NONE', #3709, #26883, #266, .T. ) ;
#25034 = AXIS2_PLACEMENT_3D ( 'NONE', #18741, #3622, #10127 ) ;
#25035 = DIRECTION ( 'NONE',  ( 1.000000000000000000, 0.000000000000000000, 0.000000000000000000 ) ) ;
#25036 = ORIENTED_EDGE ( 'NONE', *, *, #15606, .T. ) ;
#25037 = EDGE_CURVE ( 'NONE', #21046, #16610, #16012, .T. ) ;
#25038 = SPHERICAL_SURFACE ( 'NONE', #21005, 0.1003956692913385851 ) ;
#25039 = B_SPLINE_CURVE_WITH_KNOTS ( 'NONE', 3,
 ( #16167, #9359, #11497, #5427, #1330, #24478, #11921, #13613 ),
 .UNSPECIFIED., .F., .F.,
 ( 4, 2, 2, 4 ),
 ( 0.000000000000000000, 0.2500000000000000000, 0.5000000000000000000, 1.000000000000000000 ),
 .UNSPECIFIED. ) ;
#25040 = VERTEX_POINT ( 'NONE', #1238 ) ;
#25041 = VECTOR ( 'NONE', #7501, 39.37007874015748143 ) ;
#25042 = CARTESIAN_POINT ( 'NONE',  ( -0.7086614173228346081, 0.000000000000000000, 1.555118110236220597 ) ) ;
#25043 = VECTOR ( 'NONE', #10600, 39.37007874015748854 ) ;
#25044 = DIRECTION ( 'NONE',  ( 0.000000000000000000, 0.000000000000000000, 1.000000000000000000 ) ) ;
#25045 = DIRECTION ( 'NONE',  ( 0.000000000000000000, 0.000000000000000000, 1.000000000000000000 ) ) ;
#25046 = CARTESIAN_POINT ( 'NONE',  ( 0.3905379133858267737, -0.5610236220472440971, 6.870559055118111198E-17 ) ) ;
#25047 = VERTEX_POINT ( 'NONE', #7299 ) ;
#25048 = CARTESIAN_POINT ( 'NONE',  ( -0.0007595033562148819414, 0.6881885572739390167, 0.3401574803149606252 ) ) ;
#25049 = ORIENTED_EDGE ( 'NONE', *, *, #25590, .T. ) ;
#25050 = CARTESIAN_POINT ( 'NONE',  ( 0.2223167940359795647, 0.2657206863494897542, 0.1377952755905510474 ) ) ;
#25051 = DIRECTION ( 'NONE',  ( 1.000000000000000000, 0.000000000000000000, 0.000000000000000000 ) ) ;
#25052 = CARTESIAN_POINT ( 'NONE',  ( 0.000000000000000000, 0.07874015748031495954, 0.000000000000000000 ) ) ;
#25053 = CARTESIAN_POINT ( 'NONE',  ( 0.6882266799383700562, -0.3177023890156830954, -0.1184012924741053158 ) ) ;
#25054 = ORIENTED_EDGE ( 'NONE', *, *, #25456, .T. ) ;
#25055 = AXIS2_PLACEMENT_3D ( 'NONE', #4838, #16421, #9341 ) ;
#25056 = CARTESIAN_POINT ( 'NONE',  ( -0.2131049448084480213, -0.5835666837866708700, 0.2574803149606298969 ) ) ;
#25057 = LINE ( 'NONE', #19224, #13768 ) ;
#25058 = DIRECTION ( 'NONE',  ( -1.000000000000000000, 0.000000000000000000, 0.000000000000000000 ) ) ;
#25059 = LENGTH_MEASURE_WITH_UNIT ( LENGTH_MEASURE( 0.02539999999999999897 ), #22666 ) ;
#25060 = ORIENTED_EDGE ( 'NONE', *, *, #8485, .T. ) ;
#25061 = CARTESIAN_POINT ( 'NONE',  ( 0.2228126397719881469, 0.3858397471888846408, -1.934055118110236338 ) ) ;
#25062 = EDGE_CURVE ( 'NONE', #4592, #17515, #12845, .T. ) ;
#25063 = AXIS2_PLACEMENT_3D ( 'NONE', #2864, #20258, #11503 ) ;
#25064 = EDGE_CURVE ( 'NONE', #18018, #19937, #3837, .T. ) ;
#25065 = CIRCLE ( 'NONE', #12892, 0.4941010236220472751 ) ;
#25066 = ORIENTED_EDGE ( 'NONE', *, *, #21474, .T. ) ;
#25067 = EDGE_LOOP ( 'NONE', ( #399, #6227, #10348, #25338 ) ) ;
#25068 = ORIENTED_EDGE ( 'NONE', *, *, #22731, .F. ) ;
#25069 = CARTESIAN_POINT ( 'NONE',  ( 0.09842519685039366473, 0.1968503937007873850, -3.272637795275590733 ) ) ;
#25070 = DIRECTION ( 'NONE',  ( 0.000000000000000000, 0.000000000000000000, 1.000000000000000000 ) ) ;
#25071 = CARTESIAN_POINT ( 'NONE',  ( 0.5118110236220472231, 0.000000000000000000, 1.747047244094488194 ) ) ;
#25072 = AXIS2_PLACEMENT_3D ( 'NONE', #12642, #25918, #21269 ) ;
#25073 = CARTESIAN_POINT ( 'NONE',  ( -0.2956505864974143805, 0.3532288989643738719, 0.1771653543307089018 ) ) ;
#25074 = ORIENTED_EDGE ( 'NONE', *, *, #25029, .T. ) ;
#25075 = CARTESIAN_POINT ( 'NONE',  ( 0.1886891683788904650, 0.3267488823401754061, -3.100567304031762284 ) ) ;
#25076 = CARTESIAN_POINT ( 'NONE',  ( 0.3015072509068625894, 0.3596217111731054850, 0.1992150590373740204 ) ) ;
#25077 = B_SPLINE_CURVE_WITH_KNOTS ( 'NONE', 3,
 ( #20585, #9838, #8293, #10821 ),
 .UNSPECIFIED., .F., .F.,
 ( 4, 4 ),
 ( 1.006307675027575899, 1.007953978091874037 ),
 .UNSPECIFIED. ) ;
#25078 = CARTESIAN_POINT ( 'NONE',  ( -0.03937007874015747977, 0.000000000000000000, 0.000000000000000000 ) ) ;
#25079 = VERTEX_POINT ( 'NONE', #3467 ) ;
#25080 = ORIENTED_EDGE ( 'NONE', *, *, #18832, .T. ) ;
#25081 = CARTESIAN_POINT ( 'NONE',  ( -0.3792810011673199977, -0.6551894325502299887, -0.5632424446553236930 ) ) ;
#25082 = DIRECTION ( 'NONE',  ( 0.000000000000000000, 0.000000000000000000, -1.000000000000000000 ) ) ;
#25083 = CIRCLE ( 'NONE', #11546, 0.07677362204724411110 ) ;
#25084 = DIRECTION ( 'NONE',  ( 0.000000000000000000, 0.000000000000000000, -1.000000000000000000 ) ) ;
#25085 = ORIENTED_EDGE ( 'NONE', *, *, #13100, .F. ) ;
#25086 = CARTESIAN_POINT ( 'NONE',  ( 0.5869493968219645641, 0.2133897621573074832, -0.3696019098714952711 ) ) ;
#25087 = DIRECTION ( 'NONE',  ( 0.000000000000000000, 0.000000000000000000, -1.000000000000000000 ) ) ;
#25088 = CIRCLE ( 'NONE', #2540, 0.01181102362204724046 ) ;
#25089 = CARTESIAN_POINT ( 'NONE',  ( -0.1791601451668923262, -0.3102476824511486986, -3.115157480314960647 ) ) ;
#25090 = DIRECTION ( 'NONE',  ( 0.000000000000000000, -1.000000000000000000, 0.000000000000000000 ) ) ;
#25091 = CARTESIAN_POINT ( 'NONE',  ( 0.5664712772799370688, 0.9591943317212182629, -0.1917392787441815627 ) ) ;
#25092 = FACE_OUTER_BOUND ( 'NONE', #20641, .T. ) ;
#25093 = CARTESIAN_POINT ( 'NONE',  ( -0.7874015748031496509, 7.558374153346456878E-06, -2.105236220445303008 ) ) ;
#25094 = EDGE_CURVE ( 'NONE', #5696, #4089, #3702, .T. ) ;
#25095 = FACE_OUTER_BOUND ( 'NONE', #22289, .T. ) ;
#25096 = DIRECTION ( 'NONE',  ( 1.000000000000000000, 0.000000000000000000, 0.000000000000000000 ) ) ;
#25097 = DIRECTION ( 'NONE',  ( 1.000000000000000000, 0.000000000000000000, 0.000000000000000000 ) ) ;
#25098 = EDGE_CURVE ( 'NONE', #8508, #16690, #27348, .T. ) ;
#25099 = EDGE_LOOP ( 'NONE', ( #23283, #20769, #9876, #27797 ) ) ;
#25100 = CARTESIAN_POINT ( 'NONE',  ( 0.07462150385400743990, 0.5672083774005964862, 0.9399606299212601712 ) ) ;
#25101 = CARTESIAN_POINT ( 'NONE',  ( 0.3937007874015748254, 0.000000000000000000, 0.01181102362204724393 ) ) ;
#25102 = SURFACE_STYLE_FILL_AREA ( #23925 ) ;
#25103 = FACE_OUTER_BOUND ( 'NONE', #14549, .T. ) ;
#25104 = FACE_OUTER_BOUND ( 'NONE', #1554, .T. ) ;
#25105 = ORIENTED_EDGE ( 'NONE', *, *, #22479, .T. ) ;
#25106 = DIRECTION ( 'NONE',  ( 0.000000000000000000, 0.000000000000000000, 1.000000000000000000 ) ) ;
#25107 = AXIS2_PLACEMENT_3D ( 'NONE', #27496, #25364, #2727 ) ;
#25108 = FACE_BOUND ( 'NONE', #26885, .T. ) ;
#25109 = DIRECTION ( 'NONE',  ( 0.000000000000000000, 1.000000000000000000, 0.000000000000000000 ) ) ;
#25110 = VERTEX_POINT ( 'NONE', #3185 ) ;
#25111 = CIRCLE ( 'NONE', #8874, 0.2952755905511810774 ) ;
#25112 = LINE ( 'NONE', #22575, #27771 ) ;
#25113 = VERTEX_POINT ( 'NONE', #18297 ) ;
#25114 = FACE_OUTER_BOUND ( 'NONE', #3357, .T. ) ;
#25115 = ( LENGTH_UNIT ( ) NAMED_UNIT ( * ) SI_UNIT ( $, .METRE. ) ) ;
#25116 = CARTESIAN_POINT ( 'NONE',  ( 0.7874015748031496509, 0.3931603432736094361, 0.1747896609116821598 ) ) ;
#25117 = CARTESIAN_POINT ( 'NONE',  ( -0.2362204724409449064, -0.4724409448818898127, -0.8182917201112815953 ) ) ;
#25118 = FACE_OUTER_BOUND ( 'NONE', #17705, .T. ) ;
#25119 = ORIENTED_EDGE ( 'NONE', *, *, #969, .T. ) ;
#25120 = CARTESIAN_POINT ( 'NONE',  ( 0.1275996891957845991, -0.4763861460130774939, -1.550196850393700920 ) ) ;
#25121 = FACE_BOUND ( 'NONE', #12736, .T. ) ;
#25122 = ORIENTED_EDGE ( 'NONE', *, *, #4204, .F. ) ;
#25123 = ORIENTED_EDGE ( 'NONE', *, *, #7556, .T. ) ;
#25124 = ITEM_DEFINED_TRANSFORMATION ( 'NONE', 'NONE', #17441,  #11588 ) ;
#25125 = DIRECTION ( 'NONE',  ( 0.000000000000000000, 0.000000000000000000, 1.000000000000000000 ) ) ;
#25126 = CARTESIAN_POINT ( 'NONE',  ( 0.000000000000000000, 0.000000000000000000, 0.2574803149606298969 ) ) ;
#25127 = FACE_OUTER_BOUND ( 'NONE', #16604, .T. ) ;
#25128 = CARTESIAN_POINT ( 'NONE',  ( -0.4621951630817708878, 0.08130208312399901660, 0.1992150590373740204 ) ) ;
#25129 = B_SPLINE_SURFACE_WITH_KNOTS ( 'NONE', 2, 3, ( 
 ( #20877, #3486, #27383, #20599, #1251, #22866, #8036, #18314, #16643, #25254, #9715, #7751, #14550, #16364, #14256, #17063, #25539, #4070, #16782, #23575, #14961, #6330, #10697, #27665, #277, #10975, #8313, #4209, #1803, #14, #2083, #19601, #8716, #10413, #12543, #144, #21162, #8580, #19312, #12813, #16930, #25680, #6200, #17198, #6060, #21717, #14829, #25817, #6465, #25394, #2214, #23437, #15098, #14692, #12676, #10837, #19030, #21579, #21303, #1941, #17338, #23709, #10549, #4344, #19171, #12949 ),
 ( #19452, #27806, #23297, #2346, #21444, #25954, #6605, #15231, #23844, #13092, #3925, #13635, #5153, #26352, #20279, #2886, #9113, #17732, #17606, #24106, #8849, #15638, #7017, #24240, #2748, #19732, #17472, #3021, #400, #4881, #21851, #20000, #22120, #11657, #794, #2490, #4604, #20136, #13225, #651, #11382, #13495, #8982, #521, #26220, #9241, #26086, #13780, #6880, #17859, #26482, #6748, #22255, #15507, #7148, #15381, #4741, #11519, #11111, #9382, #13363, #21989, #17989, #15770, #2621, #24373 ),
 ( #5014, #26625, #7280, #11243, #23969, #22399, #19867, #15899, #24502, #27206, #16462, #20835, #12361, #5740, #25211, #18420, #937, #12222, #24791, #26919, #22828, #16047, #25075, #7563, #3166, #9525, #11799, #13924, #7855, #16190, #3591, #18708, #14357, #10098, #18278, #14508, #5454, #14067, #20419, #22969, #12082, #3304, #5880, #23110, #18125, #27066, #1081, #22679, #11947, #26769, #7716, #20566, #1217, #1487, #9821, #16328, #3741, #7417, #9677, #5302, #14219, #22541, #5591, #27344, #3446, #20702 ) ),
 .UNSPECIFIED., .F., .T., .F.,
 ( 3, 3 ),
 ( 4, 2, 2, 2, 2, 2, 2, 2, 2, 2, 2, 2, 2, 2, 2, 2, 2, 2, 2, 2, 2, 2, 2, 2, 2, 2, 2, 2, 2, 2, 2, 2, 4 ),
 ( 0.000000000000000000, 1.000000000000000000 ),
 ( 0.000000000000000000, 0.1963495408493620697, 0.3926990816987241395, 0.5890486225480862092, 0.7853981633974482790, 0.9817477042468103487, 1.178097245096172418, 1.374446785945534488, 1.570796326794896558, 1.767145867644258628, 1.963495408493620697, 2.159844949342982545, 2.356194490192344837, 2.552544031041707129, 2.748893571891068976, 2.945243112740430824, 3.141592653589793116, 3.337942194439155408, 3.534291735288517255, 3.730641276137879103, 3.926990816987241395, 4.123340357836603687, 4.319689898685965090, 4.516039439535327382, 4.712388980384689674, 4.908738521234051966, 5.105088062083414258, 5.301437602932775661, 5.497787143782137953, 5.694136684631500245, 5.890486225480861648, 6.086835766330223940, 6.283185307179586232 ),
 .UNSPECIFIED. ) ;
#25130 = ORIENTED_EDGE ( 'NONE', *, *, #8672, .F. ) ;
#25131 = CARTESIAN_POINT ( 'NONE',  ( 0.000000000000000000, 0.000000000000000000, -4.330708661417323135 ) ) ;
#25132 = B_SPLINE_CURVE_WITH_KNOTS ( 'NONE', 3,
 ( #24431, #16113, #864, #2679, #5224, #11722, #24707, #4803 ),
 .UNSPECIFIED., .F., .F.,
 ( 4, 2, 2, 4 ),
 ( 0.5000000000000000000, 0.7499999999999996669, 0.8749999999999997780, 1.000000000000000000 ),
 .UNSPECIFIED. ) ;
#25133 = ADVANCED_FACE ( 'NONE', ( #1644 ), #8014, .F. ) ;
#25134 = UNCERTAINTY_MEASURE_WITH_UNIT (LENGTH_MEASURE( 1.000000000000000082E-05 ), #14651, 'distance_accuracy_value', 'NONE') ;
#25135 = LINE ( 'NONE', #25420, #6950 ) ;
#25136 = FACE_OUTER_BOUND ( 'NONE', #21230, .T. ) ;
#25137 = CARTESIAN_POINT ( 'NONE',  ( 1.802635347151102296, -2.925196850393700920, 0.7675577426145275828 ) ) ;
#25138 = ADVANCED_FACE ( 'NONE', ( #6444 ), #9213, .F. ) ;
#25139 = CARTESIAN_POINT ( 'NONE',  ( -0.5677563751001175607, -0.3136670689571407489, 0.1974823232504523962 ) ) ;
#25140 = CARTESIAN_POINT ( 'NONE',  ( -0.03532354024591771724, -0.6299212598425196763, 0.000000000000000000 ) ) ;
#25141 = DIRECTION ( 'NONE',  ( 0.9930684569549264040, 0.05876869872891801738, -0.1017903720931950112 ) ) ;
#25142 = ORIENTED_EDGE ( 'NONE', *, *, #24991, .F. ) ;
#25143 = AXIS2_PLACEMENT_3D ( 'NONE', #3704, #24897, #14317 ) ;
#25144 = LINE ( 'NONE', #20631, #2475 ) ;
#25145 = VERTEX_POINT ( 'NONE', #8426 ) ;
#25146 = VECTOR ( 'NONE', #11226, 39.37007874015748143 ) ;
#25147 = ORIENTED_EDGE ( 'NONE', *, *, #21762, .T. ) ;
#25148 = AXIS2_PLACEMENT_3D ( 'NONE', #23534, #21401, #17160 ) ;
#25149 = CARTESIAN_POINT ( 'NONE',  ( -0.4684132450478830645, -0.1062614382955276715, 0.2362204724409449619 ) ) ;
#25150 = CARTESIAN_POINT ( 'NONE',  ( 0.1520643344662694629, 0.4930463976998556985, 0.03726710077533022109 ) ) ;
#25151 = ORIENTED_EDGE ( 'NONE', *, *, #8524, .F. ) ;
#25152 = DIRECTION ( 'NONE',  ( 0.000000000000000000, 0.000000000000000000, 1.000000000000000000 ) ) ;
#25153 = ORIENTED_EDGE ( 'NONE', *, *, #8158, .T. ) ;
#25154 = EDGE_CURVE ( 'NONE', #3990, #20420, #2476, .T. ) ;
#25155 = CARTESIAN_POINT ( 'NONE',  ( 0.1180276236025432773, -0.3257325899126712887, 0.1478915661236427093 ) ) ;
#25156 = CARTESIAN_POINT ( 'NONE',  ( -0.4599980997183342191, -0.2268967137092737507, -1.550196850393701364 ) ) ;
#25157 = CIRCLE ( 'NONE', #16134, 0.09842519685039370636 ) ;
#25158 = CARTESIAN_POINT ( 'NONE',  ( 0.000000000000000000, 0.000000000000000000, -3.278217716535432842E-17 ) ) ;
#25159 = ORIENTED_EDGE ( 'NONE', *, *, #11979, .T. ) ;
#25160 = DIRECTION ( 'NONE',  ( -1.000000000000000000, 0.000000000000000000, 0.000000000000000000 ) ) ;
#25161 = AXIS2_PLACEMENT_3D ( 'NONE', #6085, #21188, #12697 ) ;
#25162 = COLOUR_RGB ( '', 0.31764706, 0.68627451, 0.89019608) ;
#25163 = DIRECTION ( 'NONE',  ( 0.000000000000000000, 0.000000000000000000, 1.000000000000000000 ) ) ;
#25164 = DIRECTION ( 'NONE',  ( 0.000000000000000000, 0.000000000000000000, 1.000000000000000000 ) ) ;
#25165 = CARTESIAN_POINT ( 'NONE',  ( -0.5511811023622048555, -0.03607471876259069760, 0.9399606299212598381 ) ) ;
#25166 = DIRECTION ( 'NONE',  ( 1.000000000000000000, 0.000000000000000000, 0.000000000000000000 ) ) ;
#25167 = ORIENTED_EDGE ( 'NONE', *, *, #12085, .T. ) ;
#25168 = LINE ( 'NONE', #5407, #11448 ) ;
#25169 = CARTESIAN_POINT ( 'NONE',  ( 0.000000000000000000, 0.000000000000000000, 0.1322834645669291320 ) ) ;
#25170 = CARTESIAN_POINT ( 'NONE',  ( 0.2104048168823795806, -0.4354435989178285782, 0.2008762816694357189 ) ) ;
#25171 = CIRCLE ( 'NONE', #12548, 0.01377952755905510404 ) ;
#25172 = ORIENTED_EDGE ( 'NONE', *, *, #15075, .F. ) ;
#25173 = CIRCLE ( 'NONE', #27006, 0.2952755905511810774 ) ;
#25174 = VERTEX_POINT ( 'NONE', #10535 ) ;
#25175 = AXIS2_PLACEMENT_3D ( 'NONE', #8009, #23415, #10110 ) ;
#25176 = CARTESIAN_POINT ( 'NONE',  ( 1.613650215246377861, 2.644685039370078705, 0.2696115963346850664 ) ) ;
#25177 = DIRECTION ( 'NONE',  ( 0.000000000000000000, 0.000000000000000000, -1.000000000000000000 ) ) ;
#25178 = CARTESIAN_POINT ( 'NONE',  ( -0.1180276236025431524, -0.3257325899126714552, 0.1377952755905512139 ) ) ;
#25179 = CARTESIAN_POINT ( 'NONE',  ( 0.03488411621168054089, -0.5314946440730492494, 1.747047244094488416 ) ) ;
#25180 = EDGE_LOOP ( 'NONE', ( #16875, #27313, #26472, #23945 ) ) ;
#25181 = DIRECTION ( 'NONE',  ( 0.000000000000000000, 1.000000000000000000, 0.000000000000000000 ) ) ;
#25182 = VERTEX_POINT ( 'NONE', #27784 ) ;
#25183 = EDGE_CURVE ( 'NONE', #10143, #19493, #21887, .T. ) ;
#25184 = CARTESIAN_POINT ( 'NONE',  ( 0.5869493968219645641, -0.2133897621573074832, 0.3696019098714952711 ) ) ;
#25185 = CARTESIAN_POINT ( 'NONE',  ( 0.3020416211901519321, -0.1738080303474756061, 0.1166443193831429581 ) ) ;
#25186 = CARTESIAN_POINT ( 'NONE',  ( -0.06045787421035515169, 0.3092457124703104632, -3.193900699392901554 ) ) ;
#25187 = AXIS2_PLACEMENT_3D ( 'NONE', #19800, #461, #8512 ) ;
#25188 = DIRECTION ( 'NONE',  ( 0.000000000000000000, 0.000000000000000000, -1.000000000000000000 ) ) ;
#25189 = LINE ( 'NONE', #27750, #24402 ) ;
#25190 = DIRECTION ( 'NONE',  ( 0.000000000000000000, -1.000000000000000000, 0.000000000000000000 ) ) ;
#25191 = EDGE_CURVE ( 'NONE', #12210, #22329, #14917, .T. ) ;
#25192 = ORIENTED_EDGE ( 'NONE', *, *, #6770, .T. ) ;
#25193 = ( LENGTH_UNIT ( ) NAMED_UNIT ( * ) SI_UNIT ( $, .METRE. ) ) ;
#25194 = CARTESIAN_POINT ( 'NONE',  ( -0.4890020181310710812, -0.1109469068261995789, 0.1643955689325500014 ) ) ;
#25195 = DIRECTION ( 'NONE',  ( 0.000000000000000000, 0.000000000000000000, 1.000000000000000000 ) ) ;
#25196 = EDGE_CURVE ( 'NONE', #27656, #16023, #17046, .T. ) ;
#25197 = ORIENTED_EDGE ( 'NONE', *, *, #19557, .T. ) ;
#25198 = CARTESIAN_POINT ( 'NONE',  ( -0.3574975638436101444, 0.000000000000000000, -3.115157480314960647 ) ) ;
#25199 = AXIS2_PLACEMENT_3D ( 'NONE', #2363, #4622, #23592 ) ;
#25200 = ORIENTED_EDGE ( 'NONE', *, *, #16048, .F. ) ;
#25201 = CARTESIAN_POINT ( 'NONE',  ( -0.3535065162672666461, -0.2712027394948650083, -1.934055118110236338 ) ) ;
#25202 = AXIS2_PLACEMENT_3D ( 'NONE', #11583, #26688, #7349 ) ;
#25203 = CIRCLE ( 'NONE', #13475, 0.5007874015748031704 ) ;
#25204 = CARTESIAN_POINT ( 'NONE',  ( -0.4585215200179055817, 0.000000000000000000, -1.928289503579156516 ) ) ;
#25205 = ORIENTED_EDGE ( 'NONE', *, *, #18285, .F. ) ;
#25206 = CIRCLE ( 'NONE', #12577, 0.8267716535433071723 ) ;
#25207 = CARTESIAN_POINT ( 'NONE',  ( -0.4609540795476803621, -0.5358253718921779374, -0.2387683900552271810 ) ) ;
#25208 = FILL_AREA_STYLE_COLOUR ( '', #10445 ) ;
#25209 = CARTESIAN_POINT ( 'NONE',  ( -0.03478633594543723007, 0.5314960629921260393, 1.747047244094488194 ) ) ;
#25210 = ORIENTED_EDGE ( 'NONE', *, *, #16911, .F. ) ;
#25211 = CARTESIAN_POINT ( 'NONE',  ( -0.09762295995069900090, 0.3644697409450268766, -3.100567304031763172 ) ) ;
#25212 = LINE ( 'NONE', #4172, #305 ) ;
#25213 = FACE_OUTER_BOUND ( 'NONE', #16650, .T. ) ;
#25214 = CARTESIAN_POINT ( 'NONE',  ( -0.2341512108694376038, 0.2669480828848188603, 1.953740157480315043 ) ) ;
#25215 = CARTESIAN_POINT ( 'NONE',  ( 0.02576258753921166489, 0.2165354330708661457, -3.644091798679236494 ) ) ;
#25216 = VERTEX_POINT ( 'NONE', #10247 ) ;
#25217 = EDGE_CURVE ( 'NONE', #11793, #3232, #15132, .T. ) ;
#25218 = CARTESIAN_POINT ( 'NONE',  ( -0.5596283908538459695, -0.2170791976991290062, -0.2655998857763979260 ) ) ;
#25219 = AXIS2_PLACEMENT_3D ( 'NONE', #27365, #14239, #22845 ) ;
#25220 = LINE ( 'NONE', #5890, #2549 ) ;
#25221 = LINE ( 'NONE', #18852, #8305 ) ;
#25223 = CARTESIAN_POINT ( 'NONE',  ( -0.4152525734085961151, -0.3642352168756899933, 0.9399606299212598381 ) ) ;
#25222 = CARTESIAN_POINT ( 'NONE',  ( -0.09855118063547688156, -0.3667122560601323022, -3.100567304031763616 ) ) ;
#25224 = VECTOR ( 'NONE', #26011, 39.37007874015748854 ) ;
#25225 = ORIENTED_EDGE ( 'NONE', *, *, #522, .T. ) ;
#25226 = ORIENTED_EDGE ( 'NONE', *, *, #13100, .T. ) ;
#25227 = ORIENTED_EDGE ( 'NONE', *, *, #19993, .F. ) ;
#25228 = LINE ( 'NONE', #1777, #18533 ) ;
#25229 = DIRECTION ( 'NONE',  ( 0.9848077530122082424, 0.1736481776669299149, -0.000000000000000000 ) ) ;
#25230 = EDGE_CURVE ( 'NONE', #152, #4045, #18244, .T. ) ;
#25231 = EDGE_CURVE ( 'NONE', #9015, #8846, #6154, .T. ) ;
#25232 = FACE_OUTER_BOUND ( 'NONE', #9617, .T. ) ;
#25233 = VECTOR ( 'NONE', #6544, 39.37007874015748143 ) ;
#25234 = CYLINDRICAL_SURFACE ( 'NONE', #17794, 0.4986013261500205074 ) ;
#25235 = DIRECTION ( 'NONE',  ( 1.000000000000000000, 0.000000000000000000, 0.000000000000000000 ) ) ;
#25236 = EDGE_CURVE ( 'NONE', #23049, #24998, #27710, .T. ) ;
#25237 = CARTESIAN_POINT ( 'NONE',  ( 0.000000000000000000, 0.000000000000000000, -2.322834645648385710 ) ) ;
#25238 = ADVANCED_FACE ( 'NONE', ( #21287 ), #25234, .T. ) ;
#25239 = CARTESIAN_POINT ( 'NONE',  ( 0.5378064472801236118, -0.3110113600220169028, 0.2574819594177531479 ) ) ;
#25240 = ADVANCED_FACE ( 'NONE', ( #14944 ), #6986, .T. ) ;
#25241 = ORIENTED_EDGE ( 'NONE', *, *, #665, .T. ) ;
#25242 = DIRECTION ( 'NONE',  ( 0.6427876096865399180, 0.7660444431189776804, -0.000000000000000000 ) ) ;
#25243 = CARTESIAN_POINT ( 'NONE',  ( 0.3483099419446107348, 0.4538399017592875118, 0.9399606299212600602 ) ) ;
#25244 = CYLINDRICAL_SURFACE ( 'NONE', #1163, 0.3543307086367249448 ) ;
#25245 = DIRECTION ( 'NONE',  ( -0.2036417511401759362, -0.4895227362422912565, 0.8478782506317890100 ) ) ;
#25246 = AXIS2_PLACEMENT_3D ( 'NONE', #6037, #21141, #10396 ) ;
#25247 = CARTESIAN_POINT ( 'NONE',  ( -0.3267210193396165585, -0.1884333032645074957, 0.07637549214372854611 ) ) ;
#25248 = CARTESIAN_POINT ( 'NONE',  ( -0.5525004126151165096, 0.09742072959660473541, 0.1771653543307086520 ) ) ;
#25249 = CARTESIAN_POINT ( 'NONE',  ( 0.09842519685039362309, 0.2165354330708660902, -3.561112174596413826 ) ) ;
#25250 = CARTESIAN_POINT ( 'NONE',  ( -0.2173565190931825430, -0.5952284643153563648, 0.2481708550949385528 ) ) ;
#25251 = CARTESIAN_POINT ( 'NONE',  ( 0.3382184156732089830, -0.3855916753051465973, 1.766732283464566899 ) ) ;
#25252 = EDGE_LOOP ( 'NONE', ( #19858, #14292, #2336, #11938 ) ) ;
#25253 = ORIENTED_EDGE ( 'NONE', *, *, #11636, .T. ) ;
#25254 = CARTESIAN_POINT ( 'NONE',  ( -0.2362439534887433856, 0.2693339498142315325, -3.115157480314960647 ) ) ;
#25255 = ORIENTED_EDGE ( 'NONE', *, *, #25183, .T. ) ;
#25256 = DIRECTION ( 'NONE',  ( -1.000000000000000000, 0.000000000000000000, 0.000000000000000000 ) ) ;
#25257 = CARTESIAN_POINT ( 'NONE',  ( -0.0005114926878479780130, 0.3662580330841598841, 0.08455817587928993184 ) ) ;
#25258 = CARTESIAN_POINT ( 'NONE',  ( -0.3007905576423877680, -0.1482986320106428613, 1.973425196850393970 ) ) ;
#25259 = ORIENTED_EDGE ( 'NONE', *, *, #2902, .T. ) ;
#25260 = ORIENTED_EDGE ( 'NONE', *, *, #9443, .T. ) ;
#25261 = EDGE_CURVE ( 'NONE', #5673, #4739, #1576, .T. ) ;
#25262 = LINE ( 'NONE', #8448, #23342 ) ;
#25263 = FACE_BOUND ( 'NONE', #911, .T. ) ;
#25264 = ORIENTED_EDGE ( 'NONE', *, *, #21289, .F. ) ;
#25265 = ORIENTED_EDGE ( 'NONE', *, *, #12351, .F. ) ;
#25266 = ADVANCED_FACE ( 'NONE', ( #4190 ), #6036, .F. ) ;
#25267 = CIRCLE ( 'NONE', #9002, 0.3543307086367249448 ) ;
#25268 = AXIS2_PLACEMENT_3D ( 'NONE', #20614, #5505, #20187 ) ;
#25269 = ITEM_DEFINED_TRANSFORMATION ( 'NONE', 'NONE', #8869,  #11588 ) ;
#25270 = DIRECTION ( 'NONE',  ( 1.000000000000000000, 0.000000000000000000, 0.000000000000000000 ) ) ;
#25271 = CARTESIAN_POINT ( 'NONE',  ( 0.1520645003680120011, 0.4909313315697558799, 0.05587710509957802968 ) ) ;
#25272 = CARTESIAN_POINT ( 'NONE',  ( -2.184900367198595585E-17, 0.6212598425196850238, 0.2574827755769818483 ) ) ;
#25273 = EDGE_CURVE ( 'NONE', #4752, #8473, #17371, .T. ) ;
#25274 = AXIS2_PLACEMENT_3D ( 'NONE', #7648, #11593, #27002 ) ;
#25275 = VERTEX_POINT ( 'NONE', #19014 ) ;
#25276 = CARTESIAN_POINT ( 'NONE',  ( 0.000000000000000000, 0.000000000000000000, -0.05511811023622047168 ) ) ;
#25277 = ADVANCED_FACE ( 'NONE', ( #25520, #21835 ), #8832, .T. ) ;
#25278 = CARTESIAN_POINT ( 'NONE',  ( 0.1259842519685039353, 0.000000000000000000, 0.000000000000000000 ) ) ;
#25279 = DIRECTION ( 'NONE',  ( 1.000000000000000000, 0.000000000000000000, 0.000000000000000000 ) ) ;
#25280 = DIRECTION ( 'NONE',  ( 0.000000000000000000, 0.000000000000000000, 1.000000000000000000 ) ) ;
#25281 = CARTESIAN_POINT ( 'NONE',  ( -0.5960173041437835106, -0.2141719054356908680, 0.2183038118118142967 ) ) ;
#25282 = CARTESIAN_POINT ( 'NONE',  ( 0.2965233727166233235, 0.3524965443697389844, 0.1903859678001459665 ) ) ;
#25283 = DIRECTION ( 'NONE',  ( 0.000000000000000000, 1.000000000000000000, 0.000000000000000000 ) ) ;
#25284 = DIRECTION ( 'NONE',  ( -1.000000000000000000, 0.000000000000000000, 0.000000000000000000 ) ) ;
#25285 = LINE ( 'NONE', #14858, #24306 ) ;
#25286 = VECTOR ( 'NONE', #25370, 39.37007874015748143 ) ;
#25287 = ORIENTED_EDGE ( 'NONE', *, *, #14509, .T. ) ;
#25288 = ORIENTED_EDGE ( 'NONE', *, *, #5693, .T. ) ;
#25289 = ( NAMED_UNIT ( * ) SI_UNIT ( $, .STERADIAN. ) SOLID_ANGLE_UNIT ( ) ) ;
#25290 = ORIENTED_EDGE ( 'NONE', *, *, #13492, .F. ) ;
#25291 = EDGE_CURVE ( 'NONE', #24104, #8578, #19636, .T. ) ;
#25292 = CARTESIAN_POINT ( 'NONE',  ( -0.3214446924536846772, 0.3840069416942866742, 0.09685039370078740717 ) ) ;
#25293 = CARTESIAN_POINT ( 'NONE',  ( -0.06200787401574803931, 7.593774443531816960E-18, 0.5905511811023621549 ) ) ;
#25294 = CARTESIAN_POINT ( 'NONE',  ( -0.4152525734086684461, 0.3642352168757148068, 0.9202755905511811330 ) ) ;
#25295 = VERTEX_POINT ( 'NONE', #15624 ) ;
#25296 = EDGE_CURVE ( 'NONE', #10260, #5267, #8790, .T. ) ;
#25297 = DIRECTION ( 'NONE',  ( 0.000000000000000000, -1.000000000000000000, 0.000000000000000000 ) ) ;
#25298 = ORIENTED_EDGE ( 'NONE', *, *, #19338, .T. ) ;
#25299 = EDGE_CURVE ( 'NONE', #21585, #26700, #504, .T. ) ;
#25300 = CARTESIAN_POINT ( 'NONE',  ( -0.2118615749922468650, -0.5840192333899535404, 0.2574803149606298969 ) ) ;
#25301 = CARTESIAN_POINT ( 'NONE',  ( 0.000000000000000000, 0.000000000000000000, 0.1771653543307086520 ) ) ;
#25302 = FACE_OUTER_BOUND ( 'NONE', #19751, .T. ) ;
#25303 = CIRCLE ( 'NONE', #13120, 0.4055118110236220486 ) ;
#25304 = DIRECTION ( 'NONE',  ( 0.000000000000000000, -1.000000000000000000, 0.000000000000000000 ) ) ;
#25305 = ORIENTED_EDGE ( 'NONE', *, *, #25706, .F. ) ;
#25306 = DIRECTION ( 'NONE',  ( 0.000000000000000000, 0.000000000000000000, -1.000000000000000000 ) ) ;
#25307 = CARTESIAN_POINT ( 'NONE',  ( 0.4442189740298561618, -0.2564173815256141631, -1.550196850393701364 ) ) ;
#25308 = VERTEX_POINT ( 'NONE', #26070 ) ;
#25309 = ORIENTED_EDGE ( 'NONE', *, *, #18871, .F. ) ;
#25310 = CIRCLE ( 'NONE', #20851, 0.01181102362204724046 ) ;
#25311 = CARTESIAN_POINT ( 'NONE',  ( 0.1482986320106464417, 0.3007905576423925420, 1.953740157480315043 ) ) ;
#25312 = CARTESIAN_POINT ( 'NONE',  ( -0.3855916753034467903, -0.3382184156749090675, -1.550196850393700920 ) ) ;
#25313 = DIRECTION ( 'NONE',  ( 0.000000000000000000, 0.000000000000000000, -1.000000000000000000 ) ) ;
#25314 = CARTESIAN_POINT ( 'NONE',  ( -0.4539000224941007744, 0.3482225189667277343, 0.9399606299212598381 ) ) ;
#25315 = CARTESIAN_POINT ( 'NONE',  ( -0.1196556571311373357, -0.3272932875254820906, 0.1589462317892271492 ) ) ;
#25316 = ORIENTED_EDGE ( 'NONE', *, *, #27857, .T. ) ;
#25317 = CARTESIAN_POINT ( 'NONE',  ( 0.4622619257814448712, 0.08092139668561752763, 0.1992125984251968684 ) ) ;
#25318 = CARTESIAN_POINT ( 'NONE',  ( 0.1711654736996354453, 0.5043865966253979760, 1.747047244094488416 ) ) ;
#25319 = APPLICATION_CONTEXT ( 'automotive_design' ) ;
#25320 = ORIENTED_EDGE ( 'NONE', *, *, #14539, .F. ) ;
#25321 = VECTOR ( 'NONE', #9032, 39.37007874015748854 ) ;
#25322 = CARTESIAN_POINT ( 'NONE',  ( -0.4921259842519975503, -0.03220957031763956036, -1.550196850393700920 ) ) ;
#25323 = ORIENTED_EDGE ( 'NONE', *, *, #2141, .F. ) ;
#25324 = DIRECTION ( 'NONE',  ( 0.000000000000000000, 0.000000000000000000, 1.000000000000000000 ) ) ;
#25325 = FACE_OUTER_BOUND ( 'NONE', #14204, .T. ) ;
#25326 = CARTESIAN_POINT ( 'NONE',  ( -0.5776041937077627253, -0.4807970751194731163, -0.9954635886629241703 ) ) ;
#25327 = CARTESIAN_POINT ( 'NONE',  ( 0.4776900717922462625, -0.2356240016486843558, 1.747047244094488194 ) ) ;
#25328 = ORIENTED_EDGE ( 'NONE', *, *, #11322, .F. ) ;
#25329 = EDGE_CURVE ( 'NONE', #19874, #17373, #16137, .T. ) ;
#25330 = CARTESIAN_POINT ( 'NONE',  ( 0.000000000000000000, 0.3543307086614172485, 0.000000000000000000 ) ) ;
#25331 = ORIENTED_EDGE ( 'NONE', *, *, #22533, .T. ) ;
#25332 = FACE_OUTER_BOUND ( 'NONE', #25606, .T. ) ;
#25333 = CARTESIAN_POINT ( 'NONE',  ( 0.3039508883504944969, 3.722324825164276661E-17, -0.1111195235210984261 ) ) ;
#25334 = DIRECTION ( 'NONE',  ( 1.000000000000000000, 0.000000000000000000, 0.000000000000000000 ) ) ;
#25335 = DIRECTION ( 'NONE',  ( 0.7660444431189780135, 0.6427876096865393629, 0.000000000000000000 ) ) ;
#25336 = ORIENTED_EDGE ( 'NONE', *, *, #18871, .T. ) ;
#25337 = DIRECTION ( 'NONE',  ( -0.000000000000000000, 1.000000000000000000, 0.000000000000000000 ) ) ;
#25338 = ORIENTED_EDGE ( 'NONE', *, *, #19037, .F. ) ;
#25339 = FILL_AREA_STYLE ('',( #12346 ) ) ;
#25340 = CARTESIAN_POINT ( 'NONE',  ( 0.2991932138496291582, 0.3411003281196904324, -1.934055118110236338 ) ) ;
#25341 = VECTOR ( 'NONE', #13137, 39.37007874015748143 ) ;
#25342 = EDGE_CURVE ( 'NONE', #24096, #5951, #6788, .T. ) ;
#25343 = EDGE_CURVE ( 'NONE', #20180, #23029, #9110, .T. ) ;
#25344 = PRESENTATION_LAYER_ASSIGNMENT (  '', '', ( #27153 ) ) ;
#25345 = ORIENTED_EDGE ( 'NONE', *, *, #24479, .T. ) ;
#25346 = ORIENTED_EDGE ( 'NONE', *, *, #19844, .T. ) ;
#25347 = CARTESIAN_POINT ( 'NONE',  ( -0.5833277509429386498, -0.1637665899405980618, -0.2526998142065598474 ) ) ;
#25348 = DIRECTION ( 'NONE',  ( 0.000000000000000000, 0.000000000000000000, -1.000000000000000000 ) ) ;
#25349 = CARTESIAN_POINT ( 'NONE',  ( -0.5043504886477528926, -0.1712563538833036247, 1.747047244094488194 ) ) ;
#25350 = EDGE_LOOP ( 'NONE', ( #4988, #7133, #5953, #27537 ) ) ;
#25351 = EDGE_LOOP ( 'NONE', ( #13786, #18736 ) ) ;
#25352 = ORIENTED_EDGE ( 'NONE', *, *, #23215, .T. ) ;
#25353 = DIRECTION ( 'NONE',  ( 1.000000000000000000, 0.000000000000000000, 0.000000000000000000 ) ) ;
#25354 = EDGE_CURVE ( 'NONE', #4605, #18279, #21701, .T. ) ;
#25355 = DIRECTION ( 'NONE',  ( 0.7071067818211350664, 8.659560570126387438E-17, -0.7071067805519599681 ) ) ;
#25356 = PRODUCT ( 'Rear Bearing Cover', 'Rear Bearing Cover', '', ( #8437 ) ) ;
#25357 = CARTESIAN_POINT ( 'NONE',  ( 0.05811937031584422236, 0.4417502570508218263, -1.934055118110236560 ) ) ;
#25358 = CIRCLE ( 'NONE', #11380, 0.1308464566929133932 ) ;
#25359 = CARTESIAN_POINT ( 'NONE',  ( 0.3362336590883814313, -0.1141709026133623794, 1.953740157480315043 ) ) ;
#25360 = ORIENTED_EDGE ( 'NONE', *, *, #25343, .T. ) ;
#25361 = ORIENTED_EDGE ( 'NONE', *, *, #24353, .F. ) ;
#25362 = VECTOR ( 'NONE', #16103, 39.37007874015748143 ) ;
#25363 = CARTESIAN_POINT ( 'NONE',  ( -0.6247226535096832567, -0.07175300650175490957, -0.2393789016825997595 ) ) ;
#25364 = DIRECTION ( 'NONE',  ( -0.000000000000000000, -0.000000000000000000, -1.000000000000000000 ) ) ;
#25366 = CARTESIAN_POINT ( 'NONE',  ( 0.2529800193559378352, 0.5131133041953702678, 0.9399606299212598381 ) ) ;
#25365 = CARTESIAN_POINT ( 'NONE',  ( 0.0001924259990619888469, 0.4692913385826771866, 0.1992150590373740204 ) ) ;
#25367 = ORIENTED_EDGE ( 'NONE', *, *, #16658, .T. ) ;
#25368 = ORIENTED_EDGE ( 'NONE', *, *, #15227, .T. ) ;
#25369 = CARTESIAN_POINT ( 'NONE',  ( 0.5869493968219645641, 0.2133897621573074832, -0.3696019098714952711 ) ) ;
#25370 = DIRECTION ( 'NONE',  ( 0.000000000000000000, 0.000000000000000000, 1.000000000000000000 ) ) ;
#25371 = AXIS2_PLACEMENT_3D ( 'NONE', #14674, #264, #23559 ) ;
#25372 = CARTESIAN_POINT ( 'NONE',  ( 0.3102476824511487541, -0.1791601451668820011, -3.115157480314960647 ) ) ;
#25373 = LINE ( 'NONE', #16346, #9852 ) ;
#25374 = CARTESIAN_POINT ( 'NONE',  ( 0.000000000000000000, 0.000000000000000000, 0.3543307086614173040 ) ) ;
#25375 = CYLINDRICAL_SURFACE ( 'NONE', #25246, 0.4921259842519685179 ) ;
#25376 = VECTOR ( 'NONE', #22552, 39.37007874015748143 ) ;
#25377 = DIRECTION ( 'NONE',  ( 0.000000000000000000, 1.000000000000000000, 0.000000000000000000 ) ) ;
#25378 = CYLINDRICAL_SURFACE ( 'NONE', #24309, 0.06889763779527552368 ) ;
#25379 = AXIS2_PLACEMENT_3D ( 'NONE', #20532, #7962, #2989 ) ;
#25380 = ORIENTED_EDGE ( 'NONE', *, *, #5920, .T. ) ;
#25381 = CARTESIAN_POINT ( 'NONE',  ( 0.000000000000000000, 0.000000000000000000, -0.1377952755905511861 ) ) ;
#25382 = CARTESIAN_POINT ( 'NONE',  ( -0.07462095020359073294, 0.5672055940106845995, 0.9399606299212600602 ) ) ;
#25383 = EDGE_CURVE ( 'NONE', #3782, #13078, #15569, .T. ) ;
#25384 = AXIS2_PLACEMENT_3D ( 'NONE', #15486, #17452, #24220 ) ;
#25385 = ORIENTED_EDGE ( 'NONE', *, *, #16581, .T. ) ;
#25386 = ADVANCED_FACE ( 'NONE', ( #8697 ), #24572, .T. ) ;
#25387 = CARTESIAN_POINT ( 'NONE',  ( 0.3715251363271980245, 0.06498290224717499786, 0.07637795275590551769 ) ) ;
#25388 = CARTESIAN_POINT ( 'NONE',  ( 0.1378076643338767004, -0.5144970376935934508, 1.747047244094488194 ) ) ;
#25389 = CARTESIAN_POINT ( 'NONE',  ( 0.1491281042588007977, -0.4788599204499175421, -0.009432676026062585331 ) ) ;
#25390 = ADVANCED_FACE ( 'NONE', ( #11095 ), #2904, .T. ) ;
#25391 = CARTESIAN_POINT ( 'NONE',  ( 0.3855916753051394363, 0.3382184156732163660, 1.747047244094488194 ) ) ;
#25392 = ORIENTED_EDGE ( 'NONE', *, *, #2768, .F. ) ;
#25393 = VERTEX_POINT ( 'NONE', #9097 ) ;
#25394 = CARTESIAN_POINT ( 'NONE',  ( -0.02339816079119156136, -0.3574975638436101444, -3.115157480314960647 ) ) ;
#25395 = EDGE_LOOP ( 'NONE', ( #7500, #26218, #21990, #1387, #25507 ) ) ;
#25396 = EDGE_CURVE ( 'NONE', #23101, #6477, #26370, .T. ) ;
#25397 = CARTESIAN_POINT ( 'NONE',  ( -0.3998447049182095037, 0.4754871227241110332, 0.2574803149606298969 ) ) ;
#25398 = ORIENTED_EDGE ( 'NONE', *, *, #11996, .F. ) ;
#25399 = DIRECTION ( 'NONE',  ( 0.000000000000000000, -1.000000000000000000, 0.000000000000000000 ) ) ;
#25400 = DIRECTION ( 'NONE',  ( 1.000000000000000000, 0.000000000000000000, 0.000000000000000000 ) ) ;
#25401 = CARTESIAN_POINT ( 'NONE',  ( -0.2211428102655755012, 0.2521176338356572177, 1.973425196850393970 ) ) ;
#25402 = ORIENTED_EDGE ( 'NONE', *, *, #1535, .F. ) ;
#25403 = VERTEX_POINT ( 'NONE', #19983 ) ;
#25404 = CARTESIAN_POINT ( 'NONE',  ( -0.3252100150720236837, -0.3707612262533185321, -1.550196850393700920 ) ) ;
#25405 = ORIENTED_EDGE ( 'NONE', *, *, #5192, .T. ) ;
#25406 = ORIENTED_EDGE ( 'NONE', *, *, #1535, .T. ) ;
#25407 = AXIS2_PLACEMENT_3D ( 'NONE', #7024, #17348, #21998 ) ;
#25408 = EDGE_CURVE ( 'NONE', #19933, #23405, #11058, .T. ) ;
#25409 = VERTEX_POINT ( 'NONE', #9615 ) ;
#25410 = DIRECTION ( 'NONE',  ( 0.000000000000000000, 0.000000000000000000, -1.000000000000000000 ) ) ;
#25411 = CARTESIAN_POINT ( 'NONE',  ( -0.4930758245789425009, 0.08754571829529331217, 0.2574803149606298969 ) ) ;
#25412 = CARTESIAN_POINT ( 'NONE',  ( 0.000000000000000000, 0.000000000000000000, 0.4488188976377953110 ) ) ;
#25413 = ORIENTED_EDGE ( 'NONE', *, *, #11831, .F. ) ;
#25414 = FACE_BOUND ( 'NONE', #24821, .T. ) ;
#25415 = AXIS2_PLACEMENT_3D ( 'NONE', #7483, #11859, #9445 ) ;
#25416 = VERTEX_POINT ( 'NONE', #4463 ) ;
#25417 = DIRECTION ( 'NONE',  ( 1.000000000000000000, 0.000000000000000000, 0.000000000000000000 ) ) ;
#25418 = AXIS2_PLACEMENT_3D ( 'NONE', #19371, #10893, #6664 ) ;
#25419 = CARTESIAN_POINT ( 'NONE',  ( 1.197070535079588716, 0.07874015748031491790, -1.197070535079588716 ) ) ;
#25420 = CARTESIAN_POINT ( 'NONE',  ( -0.03937007874015747977, -5.785732909357575061E-17, -0.4724409448818898127 ) ) ;
#25421 = LINE ( 'NONE', #3952, #26794 ) ;
#25422 = DIRECTION ( 'NONE',  ( 0.000000000000000000, 0.000000000000000000, 1.000000000000000000 ) ) ;
#25423 = EDGE_CURVE ( 'NONE', #12635, #13218, #11129, .T. ) ;
#25424 = CARTESIAN_POINT ( 'NONE',  ( -0.4622285577935897893, 0.08111201067594607517, 0.07637630773773071424 ) ) ;
#25425 = CARTESIAN_POINT ( 'NONE',  ( -6.132876883919029269E-17, -0.5007874015748031704, 0.3543307086614173040 ) ) ;
#25426 = CARTESIAN_POINT ( 'NONE',  ( -0.09842519685039370636, -0.07874015748031495954, 0.04546065111729331171 ) ) ;
#25427 = CARTESIAN_POINT ( 'NONE',  ( -0.0003954787107570180166, 0.5007872847596378518, 0.2574819596263889787 ) ) ;
#25428 = EDGE_CURVE ( 'NONE', #21681, #19875, #21946, .T. ) ;
#25429 = AXIS2_PLACEMENT_3D ( 'NONE', #1255, #5780, #20602 ) ;
#25430 = DIRECTION ( 'NONE',  ( 1.000000000000000000, 0.000000000000000000, 0.000000000000000000 ) ) ;
#25431 = VERTEX_POINT ( 'NONE', #18221 ) ;
#25432 = CARTESIAN_POINT ( 'NONE',  ( 0.5869493968219645641, -0.2133897621573074832, 0.3696019098714952711 ) ) ;
#25433 = ORIENTED_EDGE ( 'NONE', *, *, #3674, .T. ) ;
#25434 = CONICAL_SURFACE ( 'NONE', #13685, 0.2012500529900838608, 1.047197550000000144 ) ;
#25435 = CARTESIAN_POINT ( 'NONE',  ( -0.4441657790094409863, -0.2564944395535778687, -1.550196850393700920 ) ) ;
#25436 = CARTESIAN_POINT ( 'NONE',  ( 0.5118110236220472231, 6.267877318470705905E-17, -0.01377952755905511792 ) ) ;
#25437 = CARTESIAN_POINT ( 'NONE',  ( -0.02559055118110236185, 0.6299212598425196763, 0.000000000000000000 ) ) ;
#25438 = AXIS2_PLACEMENT_3D ( 'NONE', #2644, #20440, #24126 ) ;
#25439 = CARTESIAN_POINT ( 'NONE',  ( -0.5230301363771427958, 0.1775991818008358647, 0.9202755905511811330 ) ) ;
#25440 = ORIENTED_EDGE ( 'NONE', *, *, #25762, .F. ) ;
#25441 = DIRECTION ( 'NONE',  ( 0.000000000000000000, 0.000000000000000000, 1.000000000000000000 ) ) ;
#25442 = ORIENTED_EDGE ( 'NONE', *, *, #928, .T. ) ;
#25443 = EDGE_CURVE ( 'NONE', #27631, #23414, #25018, .T. ) ;
#25444 = CARTESIAN_POINT ( 'NONE',  ( 0.5375739373539409893, 0.4296723508511047229, 0.3401574803149606252 ) ) ;
#25445 = CARTESIAN_POINT ( 'NONE',  ( -0.2181459867488315385, -0.4514914377086566288, 0.3080453759322188123 ) ) ;
#25446 = AXIS2_PLACEMENT_3D ( 'NONE', #27021, #14307, #7666 ) ;
#25447 = CARTESIAN_POINT ( 'NONE',  ( -0.1716509673353403542, -0.4704508543867079173, 0.2574819596263889787 ) ) ;
#25448 = ORIENTED_EDGE ( 'NONE', *, *, #22135, .T. ) ;
#25449 = DIRECTION ( 'NONE',  ( 1.000000000000000000, 0.000000000000000000, 0.000000000000000000 ) ) ;
#25450 = EDGE_LOOP ( 'NONE', ( #5298, #25938 ) ) ;
#25451 = CARTESIAN_POINT ( 'NONE',  ( 0.1677079028045370679, 0.2904160862623488826, 1.953740157480315043 ) ) ;
#25452 = CARTESIAN_POINT ( 'NONE',  ( 0.4856708409191126674, 0.1649135259639225026, -1.550196850393700920 ) ) ;
#25453 = DIRECTION ( 'NONE',  ( 0.9848077530122081313, 0.1736481776669301369, -0.000000000000000000 ) ) ;
#25454 = DIRECTION ( 'NONE',  ( 0.000000000000000000, 1.000000000000000000, 0.000000000000000000 ) ) ;
#25456 = EDGE_CURVE ( 'NONE', #11052, #15868, #26994, .T. ) ;
#25455 = CONICAL_SURFACE ( 'NONE', #8324, 0.1074461786882927178, 1.047197550000000144 ) ;
#25457 = CARTESIAN_POINT ( 'NONE',  ( -0.07214854559198104200, 0.5476281405333119912, 0.9399606299212598381 ) ) ;
#25458 = DIRECTION ( 'NONE',  ( 0.000000000000000000, -1.000000000000000000, 0.000000000000000000 ) ) ;
#25459 = CIRCLE ( 'NONE', #22299, 0.01181102362204724393 ) ;
#25460 = CARTESIAN_POINT ( 'NONE',  ( 0.5511811023268710086, 6.991093931924045359E-17, 1.747047244094488194 ) ) ;
#25461 = ORIENTED_EDGE ( 'NONE', *, *, #25627, .T. ) ;
#25462 = DIRECTION ( 'NONE',  ( 1.000000000000000000, 0.000000000000000000, 0.000000000000000000 ) ) ;
#25463 = ADVANCED_FACE ( 'NONE', ( #1574 ), #4287, .T. ) ;
#25464 = FACE_OUTER_BOUND ( 'NONE', #13485, .T. ) ;
#25465 = CARTESIAN_POINT ( 'NONE',  ( 0.2089723435111824623, -0.4324731448915265508, 0.2362204724409445455 ) ) ;
#25466 = ORIENTED_EDGE ( 'NONE', *, *, #19844, .F. ) ;
#25467 = VECTOR ( 'NONE', #21611, 39.37007874015748143 ) ;
#25468 = ORIENTED_EDGE ( 'NONE', *, *, #26914, .F. ) ;
#25469 = CARTESIAN_POINT ( 'NONE',  ( 0.3382184156749452608, -0.3855916753034395184, -1.550196850393700920 ) ) ;
#25470 = EDGE_CURVE ( 'NONE', #14064, #16082, #17539, .T. ) ;
#25471 = CARTESIAN_POINT ( 'NONE',  ( -0.4009292313432017418, -0.2321359940680557676, 0.1494804571774004665 ) ) ;
#25472 = DIRECTION ( 'NONE',  ( 0.000000000000000000, 0.000000000000000000, -1.000000000000000000 ) ) ;
#25473 = CARTESIAN_POINT ( 'NONE',  ( -0.1379038425970198212, -0.5144793533649091311, 1.747047244094487972 ) ) ;
#25474 = CARTESIAN_POINT ( 'NONE',  ( 0.3856568748495315946, 0.3381512095064278522, -1.550196850393701364 ) ) ;
#25475 = CARTESIAN_POINT ( 'NONE',  ( -0.5751341951449447931, -0.6192718686200742173, 0.9188498711508340522 ) ) ;
#25476 = VERTEX_POINT ( 'NONE', #12032 ) ;
#25477 = EDGE_CURVE ( 'NONE', #8591, #7932, #23697, .T. ) ;
#25478 = CIRCLE ( 'NONE', #18219, 0.4921259842519685179 ) ;
#25479 = DIRECTION ( 'NONE',  ( 0.000000000000000000, -1.000000000000000000, 0.000000000000000000 ) ) ;
#25480 = CARTESIAN_POINT ( 'NONE',  ( -0.5670365097597637183, -0.5142378326786118947, -0.9905099408301584196 ) ) ;
#25481 = AXIS2_PLACEMENT_3D ( 'NONE', #5323, #7437, #24807 ) ;
#25482 = CARTESIAN_POINT ( 'NONE',  ( 0.000000000000000000, 0.000000000000000000, 0.01181102362204724393 ) ) ;
#25483 = DIRECTION ( 'NONE',  ( 0.000000000000000000, 1.000000000000000000, 0.000000000000000000 ) ) ;
#25484 = CARTESIAN_POINT ( 'NONE',  ( 0.000000000000000000, 0.9055118110236221041, -0.3937007874015748254 ) ) ;
#25485 = EDGE_LOOP ( 'NONE', ( #11549, #17461, #15890, #26611 ) ) ;
#25486 = DIRECTION ( 'NONE',  ( 0.000000000000000000, 0.000000000000000000, 1.000000000000000000 ) ) ;
#25487 = FACE_BOUND ( 'NONE', #21300, .T. ) ;
#25488 = ORIENTED_EDGE ( 'NONE', *, *, #25064, .F. ) ;
#25489 = FILL_AREA_STYLE ('',( #16881 ) ) ;
#25490 = CARTESIAN_POINT ( 'NONE',  ( 0.4763861460130341396, -0.1275996891957698887, -1.569881889763779625 ) ) ;
#25491 = AXIS2_PLACEMENT_3D ( 'NONE', #17330, #25807, #6455 ) ;
#25492 = CARTESIAN_POINT ( 'NONE',  ( -0.3645739570812708275, 0.2796934465393700053, -1.928289503579159625 ) ) ;
#25493 = EDGE_CURVE ( 'NONE', #22371, #10946, #14301, .T. ) ;
#25494 = CARTESIAN_POINT ( 'NONE',  ( -0.2490711204941346568, 1.208528701367826752, -0.6047752023237676910 ) ) ;
#25495 = TOROIDAL_SURFACE ( 'NONE', #6543, 0.5610236220472440971, 0.1003937007874015908 ) ;
#25496 = ORIENTED_EDGE ( 'NONE', *, *, #17482, .F. ) ;
#25497 = ORIENTED_EDGE ( 'NONE', *, *, #6158, .T. ) ;
#25498 = ORIENTED_EDGE ( 'NONE', *, *, #25846, .F. ) ;
#25499 = AXIS2_PLACEMENT_3D ( 'NONE', #6376, #19367, #18683 ) ;
#25500 = CARTESIAN_POINT ( 'NONE',  ( -0.4995226175161708859, -0.5628959716349646314, 0.1069947647043326677 ) ) ;
#25501 = CARTESIAN_POINT ( 'NONE',  ( -0.06957181182499248828, -0.5280699926562971713, 1.747047244094488194 ) ) ;
#25502 = SURFACE_SIDE_STYLE ('',( #14353 ) ) ;
#25503 = ORIENTED_EDGE ( 'NONE', *, *, #9101, .T. ) ;
#25504 = CARTESIAN_POINT ( 'NONE',  ( 0.1516263115863346334, -0.2937912646890007973, 0.3972688187320929099 ) ) ;
#25505 = FACE_OUTER_BOUND ( 'NONE', #25351, .T. ) ;
#25506 = CARTESIAN_POINT ( 'NONE',  ( -0.4303681241740391905, 0.1153557615289447225, -1.934055118110236338 ) ) ;
#25507 = ORIENTED_EDGE ( 'NONE', *, *, #26490, .F. ) ;
#25508 = CARTESIAN_POINT ( 'NONE',  ( -0.09187177619658792871, 0.3429980251342187314, 1.953740157480315043 ) ) ;
#25509 = VERTEX_POINT ( 'NONE', #27010 ) ;
#25510 = CARTESIAN_POINT ( 'NONE',  ( -0.5943003644086487514, -0.1394605577792424056, -0.2482195849639082796 ) ) ;
#25511 = CARTESIAN_POINT ( 'NONE',  ( 0.0005789221761808661720, 0.4692909815006409691, 0.1992125984251968684 ) ) ;
#25512 = EDGE_LOOP ( 'NONE', ( #145, #13493, #12175, #5877 ) ) ;
#25513 = ORIENTED_EDGE ( 'NONE', *, *, #19914, .F. ) ;
#25514 = CARTESIAN_POINT ( 'NONE',  ( 0.01504182353227358389, 0.000000000000000000, 0.000000000000000000 ) ) ;
#25515 = DIRECTION ( 'NONE',  ( 1.000000000000000000, 0.000000000000000000, 0.000000000000000000 ) ) ;
#25516 = EDGE_CURVE ( 'NONE', #18462, #5530, #10140, .T. ) ;
#25517 = AXIS2_PLACEMENT_3D ( 'NONE', #14552, #14258, #26960 ) ;
#25518 = AXIS2_PLACEMENT_3D ( 'NONE', #22275, #11678, #20300 ) ;
#25519 = CARTESIAN_POINT ( 'NONE',  ( -0.2997912780622380979, -0.1736589463928937815, 0.1377952755905510751 ) ) ;
#25520 = FACE_BOUND ( 'NONE', #25666, .T. ) ;
#25521 = FACE_BOUND ( 'NONE', #24481, .T. ) ;
#25522 = CARTESIAN_POINT ( 'NONE',  ( 0.0005847768872433690111, 0.4787829797941601240, 0.1920935997050574051 ) ) ;
#25523 = VECTOR ( 'NONE', #7717, 39.37007874015748854 ) ;
#25524 = VERTEX_POINT ( 'NONE', #5826 ) ;
#25525 = CARTESIAN_POINT ( 'NONE',  ( -0.5840206614248149020, -0.4658374228744227574, -0.9954608982700227093 ) ) ;
#25526 = EDGE_CURVE ( 'NONE', #24815, #23096, #6564, .T. ) ;
#25527 = FACE_OUTER_BOUND ( 'NONE', #22519, .T. ) ;
#25528 = CIRCLE ( 'NONE', #5689, 0.07874015748031489015 ) ;
#25529 = VERTEX_POINT ( 'NONE', #18649 ) ;
#25530 = DIRECTION ( 'NONE',  ( 0.000000000000000000, 0.000000000000000000, 1.000000000000000000 ) ) ;
#25531 = DIRECTION ( 'NONE',  ( 0.000000000000000000, 0.000000000000000000, 1.000000000000000000 ) ) ;
#25532 = ORIENTED_EDGE ( 'NONE', *, *, #6335, .T. ) ;
#25533 = ORIENTED_EDGE ( 'NONE', *, *, #24700, .F. ) ;
#25534 = DIRECTION ( 'NONE',  ( 1.000000000000000000, 0.000000000000000000, 0.000000000000000000 ) ) ;
#25535 = CARTESIAN_POINT ( 'NONE',  ( 0.02576258704323635199, 0.2165354330708661457, -3.644091798884676159 ) ) ;
#25536 = CARTESIAN_POINT ( 'NONE',  ( -0.4783464566929133688, -0.4724409448818898127, -0.9954570744419902750 ) ) ;
#25537 = VERTEX_POINT ( 'NONE', #7656 ) ;
#25538 = ORIENTED_EDGE ( 'NONE', *, *, #4541, .T. ) ;
#25539 = CARTESIAN_POINT ( 'NONE',  ( -0.02339816079119098197, 0.3574975638436101444, -3.115157480314960647 ) ) ;
#25540 = AXIS2_PLACEMENT_3D ( 'NONE', #6133, #2421, #8381 ) ;
#25541 = PLANE ( 'NONE',  #16392 ) ;
#25542 = VERTEX_POINT ( 'NONE', #23202 ) ;
#25543 = ( NAMED_UNIT ( * ) SI_UNIT ( $, .STERADIAN. ) SOLID_ANGLE_UNIT ( ) ) ;
#25544 = CARTESIAN_POINT ( 'NONE',  ( -0.3065394984460679817, 0.3644188802930369842, 0.2330651857766198043 ) ) ;
#25545 = CARTESIAN_POINT ( 'NONE',  ( -0.1482986320106437217, -0.3007905576423873795, 1.973425196850393970 ) ) ;
#25546 = ORIENTED_EDGE ( 'NONE', *, *, #6631, .T. ) ;
#25547 = ORIENTED_EDGE ( 'NONE', *, *, #7278, .T. ) ;
#25548 = AXIS2_PLACEMENT_3D ( 'NONE', #10760, #15438, #23768 ) ;
#25549 = CARTESIAN_POINT ( 'NONE',  ( 0.2466292688015316592, -0.4270824798167792147, -1.550196850393700920 ) ) ;
#25550 = FACE_OUTER_BOUND ( 'NONE', #27578, .T. ) ;
#25551 = CARTESIAN_POINT ( 'NONE',  ( -0.3713448905834433322, 0.06600512665679449109, 0.1992125984251968684 ) ) ;
#25552 = ORIENTED_EDGE ( 'NONE', *, *, #14012, .T. ) ;
#25553 = VERTEX_POINT ( 'NONE', #1299 ) ;
#25554 = EDGE_LOOP ( 'NONE', ( #26039, #17739, #15001, #14419 ) ) ;
#25555 = CYLINDRICAL_SURFACE ( 'NONE', #5446, 0.1771653543307086798 ) ;
#25556 = ITEM_DEFINED_TRANSFORMATION ( 'NONE', 'NONE', #19298,  #11588 ) ;
#25557 = CARTESIAN_POINT ( 'NONE',  ( 0.000000000000000000, 0.000000000000000000, -0.2204724409448818867 ) ) ;
#25558 = CARTESIAN_POINT ( 'NONE',  ( -0.3606190329934327310, 0.4297690281277732338, 0.1771653543307086520 ) ) ;
#25559 = B_SPLINE_CURVE_WITH_KNOTS ( 'NONE', 3,
 ( #7779, #5516, #10298, #22742, #3365, #12012, #16386, #24995, #20766, #6356, #12840, #10441, #27689, #25704, #17227, #21191, #23605, #25844 ),
 .UNSPECIFIED., .F., .F.,
 ( 4, 2, 2, 2, 2, 2, 2, 2, 4 ),
 ( 0.000000000000000000, 0.06249999999999995837, 0.1249999999999999167, 0.1874999999999999167, 0.2499999999999999445, 0.3124999999999999445, 0.3749999999999999445, 0.4375000000000000000, 0.5000000000000000000 ),
 .UNSPECIFIED. ) ;
#25560 = DIRECTION ( 'NONE',  ( -0.000000000000000000, -1.000000000000000000, -0.000000000000000000 ) ) ;
#25561 = EDGE_CURVE ( 'NONE', #14369, #27683, #13327, .T. ) ;
#25562 = DIRECTION ( 'NONE',  ( 0.000000000000000000, 1.000000000000000000, 0.000000000000000000 ) ) ;
#25563 = EDGE_CURVE ( 'NONE', #22050, #23475, #23610, .T. ) ;
#25564 = CONICAL_SURFACE ( 'NONE', #26422, 0.1106489370078739681, 0.08726646250000029414 ) ;
#25565 = DIRECTION ( 'NONE',  ( 0.000000000000000000, -0.9847781868929988969, 0.1738157720684100072 ) ) ;
#25566 = CARTESIAN_POINT ( 'NONE',  ( -1.357510822077637958, -1.563633646945708833, 2.027559055118110187 ) ) ;
#25567 = CIRCLE ( 'NONE', #22841, 0.1673228346456692994 ) ;
#25568 = CARTESIAN_POINT ( 'NONE',  ( -0.6021528086661247503, -0.1927643575067814197, 0.2217236187994692798 ) ) ;
#25569 = CARTESIAN_POINT ( 'NONE',  ( -0.4006498629591500604, 0.2309201403895328464, -1.928289503579156960 ) ) ;
#25570 = DIRECTION ( 'NONE',  ( -0.000000000000000000, -0.000000000000000000, -1.000000000000000000 ) ) ;
#25571 = CARTESIAN_POINT ( 'NONE',  ( -0.5905511811023621549, 0.000000000000000000, 0.000000000000000000 ) ) ;
#25572 = CARTESIAN_POINT ( 'NONE',  ( 0.01030706208231648401, 0.1968503937007873850, -3.193897637795275912 ) ) ;
#25573 = FACE_OUTER_BOUND ( 'NONE', #21598, .T. ) ;
#25574 = ORIENTED_EDGE ( 'NONE', *, *, #8111, .F. ) ;
#25575 = ORIENTED_EDGE ( 'NONE', *, *, #15081, .F. ) ;
#25576 = CARTESIAN_POINT ( 'NONE',  ( 0.3263749705684267921, -0.1890319631540330891, 0.07637795275590551769 ) ) ;
#25577 = VERTEX_POINT ( 'NONE', #5396 ) ;
#25578 = VERTEX_POINT ( 'NONE', #26992 ) ;
#25579 = CARTESIAN_POINT ( 'NONE',  ( -0.2602238532265429005, 0.000000000000000000, 0.2362204724409449064 ) ) ;
#25580 = CIRCLE ( 'NONE', #7519, 0.4267795243146149664 ) ;
#25581 = CARTESIAN_POINT ( 'NONE',  ( 2.664928230027803213, 0.9448818897637796255, -1.639108661417322569E-17 ) ) ;
#25582 = CARTESIAN_POINT ( 'NONE',  ( 0.4954197419817656933, 0.2442565704126251624, 0.9202755905511811330 ) ) ;
#25583 = ORIENTED_EDGE ( 'NONE', *, *, #25622, .F. ) ;
#25584 = VERTEX_POINT ( 'NONE', #16407 ) ;
#25585 = EDGE_CURVE ( 'NONE', #14002, #9997, #3246, .T. ) ;
#25586 = VECTOR ( 'NONE', #19487, 39.37007874015748854 ) ;
#25587 = LINE ( 'NONE', #6242, #8654 ) ;
#25588 = CARTESIAN_POINT ( 'NONE',  ( -0.4537304931026616139, 0.07942646906834205378, 0.1771653543307086243 ) ) ;
#25589 = DIRECTION ( 'NONE',  ( 1.000000000000000000, 0.000000000000000000, 0.000000000000000000 ) ) ;
#25590 = EDGE_CURVE ( 'NONE', #16095, #218, #22761, .T. ) ;
#25591 = DIRECTION ( 'NONE',  ( -0.5000000010362839475, -0.8660254031861397417, -1.060575237992202059E-16 ) ) ;
#25592 = ORIENTED_EDGE ( 'NONE', *, *, #13911, .T. ) ;
#25593 = DIRECTION ( 'NONE',  ( 0.000000000000000000, 0.000000000000000000, -1.000000000000000000 ) ) ;
#25594 = CARTESIAN_POINT ( 'NONE',  ( 0.2420394123212937232, 0.2892587550802425134, 0.1992125984251968684 ) ) ;
#25595 = EDGE_LOOP ( 'NONE', ( #15800, #307 ) ) ;
#25596 = DIRECTION ( 'NONE',  ( -1.000000000000000000, 0.000000000000000000, 0.000000000000000000 ) ) ;
#25597 = DIRECTION ( 'NONE',  ( 0.000000000000000000, -1.000000000000000000, 0.000000000000000000 ) ) ;
#25598 = CARTESIAN_POINT ( 'NONE',  ( 0.3642352168757886366, 0.4152525734086595088, 0.9399606299212598381 ) ) ;
#25599 = ( GEOMETRIC_REPRESENTATION_CONTEXT ( 3 ) GLOBAL_UNCERTAINTY_ASSIGNED_CONTEXT ( ( #3650 ) ) GLOBAL_UNIT_ASSIGNED_CONTEXT ( ( #13265, #17890, #15670 ) ) REPRESENTATION_CONTEXT ( 'NONE', 'WORKASPACE' ) ) ;
#25600 = LINE ( 'NONE', #8775, #14181 ) ;
#25601 = EDGE_LOOP ( 'NONE', ( #25547, #15390, #552, #15947 ) ) ;
#25602 = B_SPLINE_SURFACE_WITH_KNOTS ( 'NONE', 2, 3, ( 
 ( #1702, #18785, #16687, #1563, #25439, #27567, #18933, #23344, #25294, #5956, #4250, #14589, #6104, #23193, #12583, #14738, #3823, #21345, #12445, #21057, #1981, #6368, #3971, #10590, #21205, #10453, #19072, #16967, #25582, #6237, #14874, #23482, #4112, #19215, #8481, #17102, #25721, #2530, #2126, #2255, #15550, #23750, #26263, #15139, #17241, #4783, #8759, #8894, #21761, #4648, #10742, #26395, #12992, #13276, #19772, #4925, #10877, #17379, #11152, #19357, #19492, #24151, #4385, #6925, #21622, #25857 ),
 ( #21484, #8622, #56, #6508, #21898, #2392, #13402, #188, #25996, #7058, #6652, #15278, #15422, #438, #9026, #2663, #23888, #11292, #17777, #11021, #4527, #19910, #13131, #17645, #19644, #561, #9158, #317, #17514, #26132, #6787, #24009, #15677, #24280, #16608, #3750, #12229, #23120, #26818, #22442, #24550, #11561, #24415, #10106, #24689, #15945, #10239, #18854, #2790, #11702, #5060, #26671, #20179, #11423, #20324, #7326, #2932, #25223, #840, #5202, #27499, #22164, #16752, #3067, #13681, #9429 ),
 ( #1634, #22301, #981, #3600, #7190, #9567, #20845, #8146, #13828, #18176, #8006, #7466, #16094, #18030, #5749, #13539, #14366, #22980, #1495, #18718, #27354, #25366, #20045, #5892, #14517, #26525, #12370, #20988, #696, #9286, #15808, #17899, #17308, #10951, #1914, #25927, #10525, #17445, #21694, #14663, #10385, #27776, #2321, #17039, #12790, #23683, #27639, #2053, #4317, #255, #25650, #21414, #118, #6304, #23548, #10665, #19287, #6027, #7994, #17175, #25789, #12922, #16902, #23267, #12515, #10813 ) ),
 .UNSPECIFIED., .F., .T., .F.,
 ( 3, 3 ),
 ( 4, 2, 2, 2, 2, 2, 2, 2, 2, 2, 2, 2, 2, 2, 2, 2, 2, 2, 2, 2, 2, 2, 2, 2, 2, 2, 2, 2, 2, 2, 2, 2, 4 ),
 ( 0.000000000000000000, 1.000000000000000000 ),
 ( 0.000000000000000000, 0.1963495408493620697, 0.3926990816987241395, 0.5890486225480862092, 0.7853981633974482790, 0.9817477042468103487, 1.178097245096172418, 1.374446785945534488, 1.570796326794896558, 1.767145867644258628, 1.963495408493620697, 2.159844949342982545, 2.356194490192344837, 2.552544031041707129, 2.748893571891068976, 2.945243112740430824, 3.141592653589793116, 3.337942194439155408, 3.534291735288517255, 3.730641276137879103, 3.926990816987241395, 4.123340357836603687, 4.319689898685965090, 4.516039439535327382, 4.712388980384689674, 4.908738521234051966, 5.105088062083414258, 5.301437602932775661, 5.497787143782137953, 5.694136684631500245, 5.890486225480861648, 6.086835766330223940, 6.283185307179586232 ),
 .UNSPECIFIED. ) ;
#25603 = CARTESIAN_POINT ( 'NONE',  ( 0.1516263115863346334, -0.2937912646890007973, 0.3972688187320929099 ) ) ;
#25604 = ORIENTED_EDGE ( 'NONE', *, *, #22606, .T. ) ;
#25605 = B_SPLINE_CURVE_WITH_KNOTS ( 'NONE', 3,
 ( #24623, #14051, #20680, #7695, #1333, #1201 ),
 .UNSPECIFIED., .F., .F.,
 ( 4, 2, 4 ),
 ( 0.5000000000000000000, 0.7500000000000000000, 1.000000000000000000 ),
 .UNSPECIFIED. ) ;
#25606 = EDGE_LOOP ( 'NONE', ( #594, #603, #19970, #19652 ) ) ;
#25607 = CARTESIAN_POINT ( 'NONE',  ( 0.06699507805604380806, -0.5085118447796470598, -1.550196850393700920 ) ) ;
#25608 = CARTESIAN_POINT ( 'NONE',  ( -0.5525886237719659366, -0.1481199686355886558, 0.9399606299212600602 ) ) ;
#25609 = CARTESIAN_POINT ( 'NONE',  ( 0.03008364706454716778, 0.1136516277932334562, 0.1968503937007874127 ) ) ;
#25610 = FACE_OUTER_BOUND ( 'NONE', #5993, .T. ) ;
#25611 = CARTESIAN_POINT ( 'NONE',  ( -0.4776874499715845213, -0.2356229156551546411, 1.747047244094488194 ) ) ;
#25612 = CARTESIAN_POINT ( 'NONE',  ( -0.0007856387884325044665, 0.7354206117107146001, 0.2763636194381670075 ) ) ;
#25613 = EDGE_LOOP ( 'NONE', ( #12354, #25746, #20379, #107, #4196 ) ) ;
#25614 = CONICAL_SURFACE ( 'NONE', #12524, 0.1106489370078740375, 0.08726646250000029414 ) ;
#25615 = EDGE_CURVE ( 'NONE', #2190, #10904, #19239, .T. ) ;
#25616 = CARTESIAN_POINT ( 'NONE',  ( -0.6145047846951736670, -0.6192722590599607502, -0.9188490092316486946 ) ) ;
#25617 = AXIS2_PLACEMENT_3D ( 'NONE', #1733, #10344, #25399 ) ;
#25618 = VECTOR ( 'NONE', #9096, 39.37007874015748143 ) ;
#25619 = DIRECTION ( 'NONE',  ( 0.000000000000000000, 0.000000000000000000, 1.000000000000000000 ) ) ;
#25620 = CARTESIAN_POINT ( 'NONE',  ( 3.616083068348477634E-17, 0.07874015748662489822, 0.2952755905511805778 ) ) ;
#25621 = DIRECTION ( 'NONE',  ( 0.000000000000000000, 1.000000000000000000, 0.000000000000000000 ) ) ;
#25622 = EDGE_CURVE ( 'NONE', #10511, #13062, #11510, .T. ) ;
#25623 = ORIENTED_EDGE ( 'NONE', *, *, #21093, .F. ) ;
#25624 = DIRECTION ( 'NONE',  ( 0.000000000000000000, 0.000000000000000000, -1.000000000000000000 ) ) ;
#25625 = DIRECTION ( 'NONE',  ( 0.000000000000000000, 0.000000000000000000, 1.000000000000000000 ) ) ;
#25626 = CARTESIAN_POINT ( 'NONE',  ( -0.4211031283192478991, -0.2438048970112350611, 0.09284957166442699139 ) ) ;
#25627 = EDGE_CURVE ( 'NONE', #23576, #11604, #13006, .T. ) ;
#25628 = CARTESIAN_POINT ( 'NONE',  ( 0.05926487674659523808, -0.4498374011143459472, -1.934055118110236338 ) ) ;
#25629 = CARTESIAN_POINT ( 'NONE',  ( -0.3132247436411769170, 0.3723693495138340470, 0.09284957166379273485 ) ) ;
#25630 = CIRCLE ( 'NONE', #11619, 0.02755905511811023931 ) ;
#25631 = ADVANCED_FACE ( 'NONE', ( #19082 ), #26385, .T. ) ;
#25632 = TOROIDAL_SURFACE ( 'NONE', #6245, 0.5610236220472440971, 0.1003937007874015908 ) ;
#25633 = ORIENTED_EDGE ( 'NONE', *, *, #1399, .F. ) ;
#25634 = EDGE_LOOP ( 'NONE', ( #13041, #27269, #8287, #12195 ) ) ;
#25635 = AXIS2_PLACEMENT_3D ( 'NONE', #18682, #1746, #12196 ) ;
#25636 = CARTESIAN_POINT ( 'NONE',  ( -0.6112138326843681302, -0.1020303416107446876, -0.2425959877567988310 ) ) ;
#25637 = DIRECTION ( 'NONE',  ( 0.000000000000000000, 1.000000000000000000, 0.000000000000000000 ) ) ;
#25638 = DIRECTION ( 'NONE',  ( 0.000000000000000000, 0.000000000000000000, -1.000000000000000000 ) ) ;
#25639 = ORIENTED_EDGE ( 'NONE', *, *, #12047, .T. ) ;
#25640 = CARTESIAN_POINT ( 'NONE',  ( -0.6711032387266713251, -0.1523958994812759926, 0.3401574803149606252 ) ) ;
#25641 = CARTESIAN_POINT ( 'NONE',  ( -0.3184597017669179020, -0.1570773243923554441, 1.953740157480315043 ) ) ;
#25643 = CARTESIAN_POINT ( 'NONE',  ( 0.1490609433615242285, 0.000000000000000000, 0.000000000000000000 ) ) ;
#25642 = CIRCLE ( 'NONE', #13443, 0.7874015748208159637 ) ;
#25644 = CARTESIAN_POINT ( 'NONE',  ( -0.3015072509068622009, 0.3596217111731054850, 0.1992150590373740204 ) ) ;
#25645 = ORIENTED_EDGE ( 'NONE', *, *, #14701, .F. ) ;
#25646 = CARTESIAN_POINT ( 'NONE',  ( -0.1141709026133623378, -0.3362336590883613363, 1.953740157480315043 ) ) ;
#25647 = ORIENTED_EDGE ( 'NONE', *, *, #2360, .T. ) ;
#25648 = CARTESIAN_POINT ( 'NONE',  ( -0.6109916490390459032, -0.1025144698334873039, -0.2426823708759043852 ) ) ;
#25649 = CARTESIAN_POINT ( 'NONE',  ( -0.3661417322834645272, -0.4724409448818898127, 0.8182917201112815953 ) ) ;
#25650 = CARTESIAN_POINT ( 'NONE',  ( -0.07472527936312729768, -0.5671862884094908130, 0.9399606299212598381 ) ) ;
#25651 = ORIENTED_EDGE ( 'NONE', *, *, #8711, .F. ) ;
#25652 = DIRECTION ( 'NONE',  ( -0.6427876096865396960, -0.7660444431189776804, 0.000000000000000000 ) ) ;
#25653 = EDGE_CURVE ( 'NONE', #24735, #27302, #1590, .T. ) ;
#25654 = AXIS2_PLACEMENT_3D ( 'NONE', #22989, #20582, #18727 ) ;
#25655 = EDGE_CURVE ( 'NONE', #18321, #17036, #18726, .T. ) ;
#25656 = AXIS2_PLACEMENT_3D ( 'NONE', #1275, #16673, #7777 ) ;
#25657 = CARTESIAN_POINT ( 'NONE',  ( 0.2462256503455907131, -0.2807137536170764003, -3.115157480314960647 ) ) ;
#25658 = CARTESIAN_POINT ( 'NONE',  ( 0.000000000000000000, 0.000000000000000000, 0.9055118110027171596 ) ) ;
#25659 = TOROIDAL_SURFACE ( 'NONE', #13455, 0.5610236220472440971, 0.1003937007874015908 ) ;
#25660 = CARTESIAN_POINT ( 'NONE',  ( 0.3100894960451806570, -0.1796141127308419627, 0.1805249803430634403 ) ) ;
#25661 = DIRECTION ( 'NONE',  ( -0.000000000000000000, 0.000000000000000000, -1.000000000000000000 ) ) ;
#25662 = CARTESIAN_POINT ( 'NONE',  ( 0.4300129863948120024, -0.2478439864030017314, -1.569881889763779625 ) ) ;
#25663 = CARTESIAN_POINT ( 'NONE',  ( -0.5871411979517291435, -0.4592307444200218747, -0.9950886577925481813 ) ) ;
#25665 = DIRECTION ( 'NONE',  ( 1.000000000000000000, 0.000000000000000000, 0.000000000000000000 ) ) ;
#25664 = VECTOR ( 'NONE', #6576, 39.37007874015748143 ) ;
#25666 = EDGE_LOOP ( 'NONE', ( #10595, #2096 ) ) ;
#25667 = DIRECTION ( 'NONE',  ( -1.000000000000000000, 0.000000000000000000, 0.000000000000000000 ) ) ;
#25668 = CARTESIAN_POINT ( 'NONE',  ( -0.3483115186085786741, 0.4538422614031236146, 0.9399606299212601712 ) ) ;
#25669 = VERTEX_POINT ( 'NONE', #6663 ) ;
#25670 = CARTESIAN_POINT ( 'NONE',  ( -0.1968503937007874127, 4.336421259842520449E-17, 0.09092130223458683158 ) ) ;
#25671 = CARTESIAN_POINT ( 'NONE',  ( 0.003937007874015826907, 0.09842519685039370636, 0.000000000000000000 ) ) ;
#25672 = CARTESIAN_POINT ( 'NONE',  ( 0.5118110236220472231, 0.000000000000000000, 1.766732283464566899 ) ) ;
#25673 = CARTESIAN_POINT ( 'NONE',  ( -0.3121994997597934973, 0.4069448477556333321, 1.747047244094488194 ) ) ;
#25674 = AXIS2_PLACEMENT_3D ( 'NONE', #13397, #20038, #17639 ) ;
#25675 = ORIENTED_EDGE ( 'NONE', *, *, #775, .T. ) ;
#25676 = ADVANCED_FACE ( 'NONE', ( #23761 ), #20530, .T. ) ;
#25677 = ORIENTED_EDGE ( 'NONE', *, *, #9823, .F. ) ;
#25678 = AXIS2_PLACEMENT_3D ( 'NONE', #19814, #7102, #19950 ) ;
#25680 = CARTESIAN_POINT ( 'NONE',  ( 0.2362439534887394721, -0.2693339498142455213, -3.115157480314960647 ) ) ;
#25679 = CARTESIAN_POINT ( 'NONE',  ( 0.000000000000000000, 0.000000000000000000, 0.3401574803149606252 ) ) ;
#25681 = AXIS2_PLACEMENT_3D ( 'NONE', #12527, #25097, #16351 ) ;
#25682 = ORIENTED_EDGE ( 'NONE', *, *, #8506, .F. ) ;
#25683 = ( CONVERSION_BASED_UNIT ( 'INCH', #21019 ) LENGTH_UNIT ( ) NAMED_UNIT ( #13403 ) ) ;
#25684 = CARTESIAN_POINT ( 'NONE',  ( 0.3561571326799479742, 1.031746018571391810, -0.5821543563138212862 ) ) ;
#25685 = CARTESIAN_POINT ( 'NONE',  ( 0.3175540113612325133, 0.1078280746903942239, 1.973425196850393970 ) ) ;
#25686 = ORIENTED_EDGE ( 'NONE', *, *, #24868, .T. ) ;
#25687 = ORIENTED_EDGE ( 'NONE', *, *, #13018, .T. ) ;
#25688 = CARTESIAN_POINT ( 'NONE',  ( 0.4423390553432928751, 0.2180862235769577551, -1.550196850393700920 ) ) ;
#25689 = CONICAL_SURFACE ( 'NONE', #2168, 0.08876456692913387014, 0.7853981624999977207 ) ;
#25690 = ORIENTED_EDGE ( 'NONE', *, *, #14743, .T. ) ;
#25691 = VERTEX_POINT ( 'NONE', #15294 ) ;
#25692 = VERTEX_POINT ( 'NONE', #23356 ) ;
#25693 = CARTESIAN_POINT ( 'NONE',  ( -0.1715719712211479508, -0.4696414150086907768, 0.1496602734581923833 ) ) ;
#25694 = CONTEXT_DEPENDENT_SHAPE_REPRESENTATION ( #6028, #24709 ) ;
#25695 = CARTESIAN_POINT ( 'NONE',  ( 0.4563908000639795848, 0.6818102780176417133, -0.6021022548815945230 ) ) ;
#25696 = CARTESIAN_POINT ( 'NONE',  ( -0.4622619257814448712, 0.08092139668561793009, 0.1992125984251968684 ) ) ;
#25697 = FACE_OUTER_BOUND ( 'NONE', #9530, .T. ) ;
#25698 = TOROIDAL_SURFACE ( 'NONE', #19842, 0.4325730547867440712, 0.01377952755905511792 ) ;
#25699 = CARTESIAN_POINT ( 'NONE',  ( -0.6710470464557933834, -0.1526433524318242252, 0.1322818203437344520 ) ) ;
#25700 = AXIS2_PLACEMENT_3D ( 'NONE', #5768, #14537, #14389 ) ;
#25701 = CARTESIAN_POINT ( 'NONE',  ( 0.5925575908939920700, 0.2268709785195988371, 0.3929520615588121824 ) ) ;
#25702 = DIRECTION ( 'NONE',  ( -1.000000000000000078E-15, 1.000000000000000000, 0.000000000000000000 ) ) ;
#25703 = CARTESIAN_POINT ( 'NONE',  ( 0.3666644560843329015, 0.2817828961649157526, -1.928289503579156294 ) ) ;
#25704 = CARTESIAN_POINT ( 'NONE',  ( 0.3935368318888682326, 0.3024344094364738167, -1.569881889763779625 ) ) ;
#25705 = DIRECTION ( 'NONE',  ( 0.000000000000000000, 0.000000000000000000, -1.000000000000000000 ) ) ;
#25706 = EDGE_CURVE ( 'NONE', #17590, #22723, #22784, .T. ) ;
#25707 = ADVANCED_FACE ( 'NONE', ( #21635 ), #1442, .T. ) ;
#25708 = CARTESIAN_POINT ( 'NONE',  ( 0.09842519685039363697, 0.2165354330708661457, -3.272637795275590733 ) ) ;
#25709 = ORIENTED_EDGE ( 'NONE', *, *, #2642, .F. ) ;
#25710 = LINE ( 'NONE', #6362, #1337 ) ;
#25711 = ( NAMED_UNIT ( * ) SI_UNIT ( $, .STERADIAN. ) SOLID_ANGLE_UNIT ( ) ) ;
#25712 = EDGE_CURVE ( 'NONE', #2591, #24815, #13463, .T. ) ;
#25713 = DIRECTION ( 'NONE',  ( -1.224646799147353207E-16, 1.000000000000000000, 0.000000000000000000 ) ) ;
#25714 = VECTOR ( 'NONE', #20327, 39.37007874015748854 ) ;
#25715 = EDGE_LOOP ( 'NONE', ( #24903, #23962 ) ) ;
#25716 = CIRCLE ( 'NONE', #38, 0.4803149606299212393 ) ;
#25717 = CARTESIAN_POINT ( 'NONE',  ( -0.3224687058348476576, 0.000000000000000000, -0.1559029880880275776 ) ) ;
#25718 = DIRECTION ( 'NONE',  ( -1.000000000000000000, 0.000000000000000000, 0.000000000000000000 ) ) ;
#25719 = EDGE_CURVE ( 'NONE', #8867, #20727, #17809, .T. ) ;
#25720 = CYLINDRICAL_SURFACE ( 'NONE', #8086, 0.1082677165354330728 ) ;
#25721 = CARTESIAN_POINT ( 'NONE',  ( 0.5230301363771282519, -0.1775991818008710588, 0.9202755905511811330 ) ) ;
#25722 = VERTEX_POINT ( 'NONE', #10605 ) ;
#25723 = CARTESIAN_POINT ( 'NONE',  ( 0.3713448905834433322, 0.06600512665679410251, 0.1992125984251968684 ) ) ;
#25724 = EDGE_LOOP ( 'NONE', ( #2548, #23828, #13979, #4345 ) ) ;
#25725 = DIRECTION ( 'NONE',  ( 1.000000000000000000, 0.000000000000000000, 0.000000000000000000 ) ) ;
#25726 = TOROIDAL_SURFACE ( 'NONE', #21671, 0.6751968503937006982, 0.01377952755905511792 ) ;
#25727 = CYLINDRICAL_SURFACE ( 'NONE', #1879, 0.5118110236220472231 ) ;
#25728 = DIRECTION ( 'NONE',  ( 0.000000000000000000, -1.000000000000000000, 0.000000000000000000 ) ) ;
#25729 = FACE_OUTER_BOUND ( 'NONE', #1910, .T. ) ;
#25730 = FACE_OUTER_BOUND ( 'NONE', #19067, .T. ) ;
#25731 = ORIENTED_EDGE ( 'NONE', *, *, #15884, .F. ) ;
#25732 = CARTESIAN_POINT ( 'NONE',  ( 0.1447526197146039584, -0.3977045540727763839, 0.1377952755905511861 ) ) ;
#25733 = DIRECTION ( 'NONE',  ( 1.000000000000000000, 0.000000000000000000, 0.000000000000000000 ) ) ;
#25734 = ORIENTED_EDGE ( 'NONE', *, *, #27574, .F. ) ;
#25735 = CARTESIAN_POINT ( 'NONE',  ( 0.000000000000000000, 0.07874015748031495954, -1.692913385826771533 ) ) ;
#25736 = AXIS2_PLACEMENT_3D ( 'NONE', #21099, #27749, #3715 ) ;
#25737 = CARTESIAN_POINT ( 'NONE',  ( 0.003937007874015826907, -4.393043307086613241E-18, 0.000000000000000000 ) ) ;
#25738 = CIRCLE ( 'NONE', #22113, 0.1003937007874015908 ) ;
#25739 = CARTESIAN_POINT ( 'NONE',  ( 0.5511811023622048555, 0.03607471876262481614, 0.9399606299212598381 ) ) ;
#25740 = B_SPLINE_CURVE_WITH_KNOTS ( 'NONE', 3,
 ( #6700, #4442, #11201, #484, #10646, #13052, #12908, #103, #21534, #17155 ),
 .UNSPECIFIED., .F., .F.,
 ( 4, 2, 2, 2, 4 ),
 ( 0.000000000000000000, 0.2500000000000000000, 0.5000000000000000000, 0.7500000000000000000, 1.000000000000000000 ),
 .UNSPECIFIED. ) ;
#25741 = FACE_BOUND ( 'NONE', #21614, .T. ) ;
#25742 = VERTEX_POINT ( 'NONE', #8497 ) ;
#25743 = CARTESIAN_POINT ( 'NONE',  ( -0.3102804211135531398, 0.1791085948259530103, -3.115157480314961091 ) ) ;
#25744 = EDGE_CURVE ( 'NONE', #22680, #25818, #17118, .T. ) ;
#25745 = PRESENTATION_LAYER_ASSIGNMENT (  '', '', ( #2279 ) ) ;
#25746 = ORIENTED_EDGE ( 'NONE', *, *, #8401, .T. ) ;
#25747 = EDGE_CURVE ( 'NONE', #22736, #17040, #23942, .T. ) ;
#25748 = EDGE_CURVE ( 'NONE', #2247, #3630, #12835, .T. ) ;
#25749 = ORIENTED_EDGE ( 'NONE', *, *, #13304, .F. ) ;
#25750 = CARTESIAN_POINT ( 'NONE',  ( 0.4954415918535722829, 0.1327036767636095571, -1.550196850393700920 ) ) ;
#25751 = DIRECTION ( 'NONE',  ( -1.000000000000000000, 0.000000000000000000, 0.000000000000000000 ) ) ;
#25752 = EDGE_CURVE ( 'NONE', #14114, #12366, #397, .T. ) ;
#25753 = DIRECTION ( 'NONE',  ( -1.000000000000000000, 0.000000000000000000, 0.000000000000000000 ) ) ;
#25754 = CARTESIAN_POINT ( 'NONE',  ( 0.4339912984563291110, -0.2498791196563492356, 0.09685039370078740717 ) ) ;
#25755 = CARTESIAN_POINT ( 'NONE',  ( -0.5144765700550301135, -0.1379032889622909541, 1.747047244094488194 ) ) ;
#25756 = CARTESIAN_POINT ( 'NONE',  ( -0.2428345617565149384, 0.2885915454824177218, 0.1992125984251968684 ) ) ;
#25757 = ORIENTED_EDGE ( 'NONE', *, *, #26360, .F. ) ;
#25758 = CARTESIAN_POINT ( 'NONE',  ( -0.2988215684304370012, -0.6199272547993012195, 0.1322810039474933141 ) ) ;
#25759 = DIRECTION ( 'NONE',  ( 0.000000000000000000, -1.000000000000000000, 0.000000000000000000 ) ) ;
#25760 = CARTESIAN_POINT ( 'NONE',  ( 1.692913385826771533, 0.4724409448818898127, 3.109831496062992451E-16 ) ) ;
#25761 = VERTEX_POINT ( 'NONE', #20336 ) ;
#25762 = EDGE_CURVE ( 'NONE', #27393, #3892, #1143, .T. ) ;
#25763 = AXIS2_PLACEMENT_3D ( 'NONE', #18415, #15766, #7413 ) ;
#25764 = DIRECTION ( 'NONE',  ( 0.000000000000000000, 0.000000000000000000, 1.000000000000000000 ) ) ;
#25765 = B_SPLINE_CURVE_WITH_KNOTS ( 'NONE', 3,
 ( #20745, #5632, #5778, #16496 ),
 .UNSPECIFIED., .F., .F.,
 ( 4, 4 ),
 ( -0.5999999999999999778, 0.000000000000000000 ),
 .UNSPECIFIED. ) ;
#25766 = VERTEX_POINT ( 'NONE', #8903 ) ;
#25767 = CARTESIAN_POINT ( 'NONE',  ( -0.4921259842519685179, 0.000000000000000000, -1.550196850393700920 ) ) ;
#25768 = DIRECTION ( 'NONE',  ( 1.000000000000000000, 0.000000000000000000, 0.000000000000000000 ) ) ;
#25769 = CARTESIAN_POINT ( 'NONE',  ( 0.2268989272875507057, -0.3929158813954434226, -1.934055118110236338 ) ) ;
#25770 = CARTESIAN_POINT ( 'NONE',  ( -0.1968503937007874127, -1.676732283464567127E-17, -0.09092130223458683158 ) ) ;
#25771 = EDGE_CURVE ( 'NONE', #19740, #7963, #27309, .T. ) ;
#25772 = VECTOR ( 'NONE', #9503, 39.37007874015748143 ) ;
#25773 = ORIENTED_EDGE ( 'NONE', *, *, #33, .T. ) ;
#25774 = CARTESIAN_POINT ( 'NONE',  ( -0.4769977115679039370, -0.4895060576974945010, -0.2102905228215523614 ) ) ;
#25775 = ( LENGTH_UNIT ( ) NAMED_UNIT ( * ) SI_UNIT ( $, .METRE. ) ) ;
#25776 = CARTESIAN_POINT ( 'NONE',  ( 0.1712563538833069832, -0.5043504886477723215, 1.747047244094488194 ) ) ;
#25777 = EDGE_CURVE ( 'NONE', #11373, #13503, #16034, .T. ) ;
#25778 = DIRECTION ( 'NONE',  ( 1.000000000000000000, 0.000000000000000000, 0.000000000000000000 ) ) ;
#25779 = ORIENTED_EDGE ( 'NONE', *, *, #25615, .F. ) ;
#25780 = CYLINDRICAL_SURFACE ( 'NONE', #20560, 1.131889763779527547 ) ;
#25781 = CIRCLE ( 'NONE', #23486, 0.3771653543307086909 ) ;
#25782 = DIRECTION ( 'NONE',  ( 0.000000000000000000, 0.000000000000000000, -1.000000000000000000 ) ) ;
#25783 = CARTESIAN_POINT ( 'NONE',  ( -0.05811992390534824471, 0.4417530401346466129, -1.934055118110236338 ) ) ;
#25784 = CARTESIAN_POINT ( 'NONE',  ( -0.6996199877990079141, 0.1397441489511527524, 0.07022294643182264151 ) ) ;
#25785 = ORIENTED_EDGE ( 'NONE', *, *, #17291, .F. ) ;
#25786 = CARTESIAN_POINT ( 'NONE',  ( -0.4446020952038907681, -0.02909913904661340714, -1.934055118110236338 ) ) ;
#25787 = CARTESIAN_POINT ( 'NONE',  ( -0.5329937562553743735, -0.2781466909400371335, -0.2850623042816753383 ) ) ;
#25788 = CARTESIAN_POINT ( 'NONE',  ( -0.5572789388079989470, -0.3225230913464889881, 0.2359405056214250451 ) ) ;
#25789 = CARTESIAN_POINT ( 'NONE',  ( -0.5131133041954075713, -0.2529800193559338384, 0.9399606299212598381 ) ) ;
#25790 = CARTESIAN_POINT ( 'NONE',  ( 0.1120675189988346587, -0.5599717622282432972, -0.2558308786799976531 ) ) ;
#25791 = DIRECTION ( 'NONE',  ( -1.000000000000000000, 0.000000000000000000, 0.000000000000000000 ) ) ;
#25792 = AXIS2_PLACEMENT_3D ( 'NONE', #23550, #8959, #11633 ) ;
#25793 = CARTESIAN_POINT ( 'NONE',  ( -0.2272836761397795113, -0.2962590301041581053, -3.115157480314960647 ) ) ;
#25794 = CARTESIAN_POINT ( 'NONE',  ( -0.5511811023622047445, 0.000000000000000000, 0.000000000000000000 ) ) ;
#25795 = DIRECTION ( 'NONE',  ( -1.000000000000000000, 0.000000000000000000, 0.000000000000000000 ) ) ;
#25796 = CARTESIAN_POINT ( 'NONE',  ( 0.2997912780622380424, -0.1736589463928938648, 0.1478915661253835667 ) ) ;
#25797 = PLANE ( 'NONE',  #20732 ) ;
#25798 = SHAPE_REPRESENTATION ( 'Shaft Seal 15x26x7', ( #11588 ), #6215 ) ;
#25799 = AXIS2_PLACEMENT_3D ( 'NONE', #2396, #13279, #17383 ) ;
#25800 = CARTESIAN_POINT ( 'NONE',  ( 0.0005980912172697295821, 0.4999996422873388968, 0.1259302777261152306 ) ) ;
#25801 = EDGE_LOOP ( 'NONE', ( #21727, #10423, #10650, #23854, #8299 ) ) ;
#25802 = FACE_BOUND ( 'NONE', #15764, .T. ) ;
#25803 = DIRECTION ( 'NONE',  ( -0.000000000000000000, -0.000000000000000000, -1.000000000000000000 ) ) ;
#25804 = ADVANCED_FACE ( 'NONE', ( #6940 ), #15562, .F. ) ;
#25805 = ORIENTED_EDGE ( 'NONE', *, *, #18832, .F. ) ;
#25806 = ORIENTED_EDGE ( 'NONE', *, *, #20927, .T. ) ;
#25807 = DIRECTION ( 'NONE',  ( 0.000000000000000000, 0.000000000000000000, 1.000000000000000000 ) ) ;
#25808 = CARTESIAN_POINT ( 'NONE',  ( 0.4690668203920866919, 0.08212126673946905375, 0.1212655228496834631 ) ) ;
#25809 = CARTESIAN_POINT ( 'NONE',  ( -0.2268096725222457366, -0.4600326175560556230, 1.766732283464566899 ) ) ;
#25810 = EDGE_CURVE ( 'NONE', #24839, #19463, #11074, .T. ) ;
#25811 = CARTESIAN_POINT ( 'NONE',  ( -0.4600326175560703335, -0.2268096725222389642, 1.747047244094488194 ) ) ;
#25812 = CARTESIAN_POINT ( 'NONE',  ( 0.1638952246732497953, -0.2749627978706437048, 0.4762495361032464958 ) ) ;
#25813 = EDGE_LOOP ( 'NONE', ( #7443, #22732, #189, #13854 ) ) ;
#25814 = AXIS2_PLACEMENT_3D ( 'NONE', #21631, #19501, #26003 ) ;
#25815 = ORIENTED_EDGE ( 'NONE', *, *, #6709, .T. ) ;
#25817 = CARTESIAN_POINT ( 'NONE',  ( 0.04679574315772527804, -0.3551931031211721379, -3.115157480314960647 ) ) ;
#25816 = DIRECTION ( 'NONE',  ( -0.2036417511401758251, 0.4895227362422921447, 0.8478782506317885659 ) ) ;
#25818 = VERTEX_POINT ( 'NONE', #19921 ) ;
#25819 = ORIENTED_EDGE ( 'NONE', *, *, #23839, .T. ) ;
#25820 = DIRECTION ( 'NONE',  ( 0.000000000000000000, 0.000000000000000000, -1.000000000000000000 ) ) ;
#25821 = ( NAMED_UNIT ( * ) SI_UNIT ( $, .STERADIAN. ) SOLID_ANGLE_UNIT ( ) ) ;
#25822 = FACE_OUTER_BOUND ( 'NONE', #2383, .T. ) ;
#25823 = CARTESIAN_POINT ( 'NONE',  ( 0.3346456692913385988, 0.000000000000000000, 1.973425196850393970 ) ) ;
#25824 = EDGE_LOOP ( 'NONE', ( #11769, #4641, #12144, #207 ) ) ;
#25825 = VERTEX_POINT ( 'NONE', #7070 ) ;
#25826 = VECTOR ( 'NONE', #8201, 39.37007874015748143 ) ;
#25827 = DIRECTION ( 'NONE',  ( 0.000000000000000000, 0.000000000000000000, -1.000000000000000000 ) ) ;
#25828 = FACE_OUTER_BOUND ( 'NONE', #14801, .T. ) ;
#25829 = ORIENTED_EDGE ( 'NONE', *, *, #10300, .F. ) ;
#25830 = ORIENTED_EDGE ( 'NONE', *, *, #24056, .T. ) ;
#25831 = EDGE_LOOP ( 'NONE', ( #26621, #24979, #14506, #22671 ) ) ;
#25832 = CARTESIAN_POINT ( 'NONE',  ( -0.3412792617076848001, 0.05967164814832656705, 0.1478915661216427813 ) ) ;
#25833 = CARTESIAN_POINT ( 'NONE',  ( 0.000000000000000000, 0.000000000000000000, -0.1111195235210984261 ) ) ;
#25834 = CARTESIAN_POINT ( 'NONE',  ( 0.8267716535433071723, 0.000000000000000000, 0.4488188976377953110 ) ) ;
#25835 = EDGE_LOOP ( 'NONE', ( #13364, #1499, #16567, #14453, #6507, #7970 ) ) ;
#25836 = PRODUCT ( 'Deep Groove Ball Bearing 20x42x12', 'Deep Groove Ball Bearing 20x42x12', '', ( #5444 ) ) ;
#25837 = AXIS2_PLACEMENT_3D ( 'NONE', #9637, #14185, #5419 ) ;
#25838 = CIRCLE ( 'NONE', #24913, 0.003937007874015741038 ) ;
#25839 = CARTESIAN_POINT ( 'NONE',  ( -0.3937007874015748254, 4.821444091131312140E-17, -3.115157480314960647 ) ) ;
#25840 = ITEM_DEFINED_TRANSFORMATION ( 'NONE', 'NONE', #20176,  #11588 ) ;
#25841 = CARTESIAN_POINT ( 'NONE',  ( 0.0002199787722625489263, 0.6212598425196850238, 0.2574827755769818483 ) ) ;
#25842 = CARTESIAN_POINT ( 'NONE',  ( -0.5905511811023621549, 1.087444635826771533, 0.1051828227901525498 ) ) ;
#25843 = CARTESIAN_POINT ( 'NONE',  ( -0.2362204724409449064, 1.131889763779527547, 0.000000000000000000 ) ) ;
#25844 = CARTESIAN_POINT ( 'NONE',  ( 0.4921259842519685179, 2.987958743070287587E-17, -1.569881889763779625 ) ) ;
#25845 = CARTESIAN_POINT ( 'NONE',  ( -0.03937007874015747977, 0.000000000000000000, 0.4724409448818898127 ) ) ;
#25846 = EDGE_CURVE ( 'NONE', #22124, #2487, #2923, .T. ) ;
#25847 = CARTESIAN_POINT ( 'NONE',  ( -0.01288382760289588647, 0.1968503937007873850, -3.174212598425197207 ) ) ;
#25848 = ORIENTED_EDGE ( 'NONE', *, *, #21441, .T. ) ;
#25849 = CARTESIAN_POINT ( 'NONE',  ( -0.2992781133269515892, -0.6197069291944330427, 0.3401574803149606252 ) ) ;
#25850 = ( LENGTH_UNIT ( ) NAMED_UNIT ( * ) SI_UNIT ( $, .METRE. ) ) ;
#25851 = AXIS2_PLACEMENT_3D ( 'NONE', #530, #4750, #21726 ) ;
#25852 = EDGE_LOOP ( 'NONE', ( #27322, #17864 ) ) ;
#25853 = CIRCLE ( 'NONE', #21342, 0.1308464566929133932 ) ;
#25854 = DIRECTION ( 'NONE',  ( 1.000000000000000000, 0.000000000000000000, 0.000000000000000000 ) ) ;
#25855 = CARTESIAN_POINT ( 'NONE',  ( 0.0007683673429997494230, 0.7042519390024098991, 0.1443310008632817665 ) ) ;
#25856 = ORIENTED_EDGE ( 'NONE', *, *, #24298, .F. ) ;
#25857 = CARTESIAN_POINT ( 'NONE',  ( -0.5511811023622047445, 0.000000000000000000, 0.9202755905511811330 ) ) ;
#25858 = AXIS2_PLACEMENT_3D ( 'NONE', #6467, #23971, #13496 ) ;
#25859 = DIMENSIONAL_EXPONENTS ( 1.000000000000000000, 0.000000000000000000, 0.000000000000000000, 0.000000000000000000, 0.000000000000000000, 0.000000000000000000, 0.000000000000000000 ) ;
#25860 = CARTESIAN_POINT ( 'NONE',  ( 0.3759206409296170226, 0.2989751379763687655, 0.2529987172494035375 ) ) ;
#25861 = ORIENTED_EDGE ( 'NONE', *, *, #26340, .F. ) ;
#25862 = DIRECTION ( 'NONE',  ( 0.000000000000000000, 0.000000000000000000, 1.000000000000000000 ) ) ;
#25863 = AXIS2_PLACEMENT_3D ( 'NONE', #17909, #11718, #1139 ) ;
#25864 = CARTESIAN_POINT ( 'NONE',  ( -0.2362204724225640262, 2.892866454453686688E-17, -4.291338582656260670 ) ) ;
#25865 = CARTESIAN_POINT ( 'NONE',  ( 0.3056525133794348315, 0.3651631491574845456, 0.2330651858023968237 ) ) ;
#25866 = FACE_OUTER_BOUND ( 'NONE', #12091, .T. ) ;
#25867 = CARTESIAN_POINT ( 'NONE',  ( -0.3856568748491470133, -0.3381512095065993262, -1.550196850393700920 ) ) ;
#25868 = CARTESIAN_POINT ( 'NONE',  ( -0.0005057506112066535546, 0.6881888373222776467, 0.1322818203437346463 ) ) ;
#25869 = EDGE_CURVE ( 'NONE', #11023, #5524, #6099, .T. ) ;
#25870 = DIRECTION ( 'NONE',  ( 0.000000000000000000, 0.000000000000000000, 1.000000000000000000 ) ) ;
#25871 = CARTESIAN_POINT ( 'NONE',  ( -0.09842519685039370636, 0.2165354330708661457, -3.456364829396327831 ) ) ;
#25872 = CARTESIAN_POINT ( 'NONE',  ( 0.4716107359567087154, 0.08256389912760109251, 0.1920935997017693131 ) ) ;
#25873 = DIRECTION ( 'NONE',  ( 0.000000000000000000, 1.000000000000000000, 0.000000000000000000 ) ) ;
#25874 = DIRECTION ( 'NONE',  ( 0.000000000000000000, 0.000000000000000000, 1.000000000000000000 ) ) ;
#25875 = CLOSED_SHELL ( 'NONE', ( #17756, #3469, #13438, #13741, #9777, #17415, #18943, #7854, #23075, #8987, #1318, #15344, #10397, #16962, #12695, #230, #2617, #2539, #22912, #19400, #13272, #4342, #5365, #8022, #18412, #5723, #21925, #12447, #16464, #8994, #2445, #13378, #9616, #13171, #17600, #24175, #4305, #24660, #14166, #5110, #18148, #17322, #16493, #19381, #21241, #19430, #18978, #18962, #6774, #3900, #26420, #18267, #10432, #21832, #27437, #7428, #24666, #24607, #4419, #23040, #26092, #23560, #8950, #14435, #509, #635, #4230, #23465, #2666, #23581, #20408, #14900 ) ) ;
#25876 = CARTESIAN_POINT ( 'NONE',  ( -0.0005789221761808661720, 0.4692909815006409691, 0.1992125984251968684 ) ) ;
#25877 = DIRECTION ( 'NONE',  ( -1.000000000000000000, 0.000000000000000000, 0.000000000000000000 ) ) ;
#25878 = AXIS2_PLACEMENT_3D ( 'NONE', #9326, #17936, #1020 ) ;
#25879 = CARTESIAN_POINT ( 'NONE',  ( -0.1839420097223181394, -0.5417097841048805762, 0.9399606299212598381 ) ) ;
#25880 = EDGE_CURVE ( 'NONE', #10004, #15380, #15584, .T. ) ;
#25881 = DIRECTION ( 'NONE',  ( -0.000000000000000000, -1.000000000000000000, -0.000000000000000000 ) ) ;
#25882 = ORIENTED_EDGE ( 'NONE', *, *, #11383, .T. ) ;
#25883 = FACE_OUTER_BOUND ( 'NONE', #1391, .T. ) ;
#25884 = AXIS2_PLACEMENT_3D ( 'NONE', #23712, #11384, #6609 ) ;
#25885 = CIRCLE ( 'NONE', #22725, 0.3031496062992122820 ) ;
#25886 = TOROIDAL_SURFACE ( 'NONE', #12345, 0.3722026523000413478, 0.02755905511811023584 ) ;
#25887 = ORIENTED_EDGE ( 'NONE', *, *, #20391, .T. ) ;
#25888 = ORIENTED_EDGE ( 'NONE', *, *, #23660, .T. ) ;
#25889 = CARTESIAN_POINT ( 'NONE',  ( 0.1649135259639241124, 0.4856708409191630715, -1.550196850393700920 ) ) ;
#25890 = CARTESIAN_POINT ( 'NONE',  ( 0.1838434515533423907, -0.5417490723641140704, 0.9399606299212598381 ) ) ;
#25891 = CARTESIAN_POINT ( 'NONE',  ( 0.3149606299212598381, 3.857155272905049219E-17, -0.03543307086614204404 ) ) ;
#25892 = FACE_OUTER_BOUND ( 'NONE', #18776, .T. ) ;
#25893 = ORIENTED_EDGE ( 'NONE', *, *, #18319, .T. ) ;
#25894 = CLOSED_SHELL ( 'NONE', ( #12995, #10258, #12600, #25238, #21803, #7043, #7657, #25463, #21225, #17925, #5488, #11352, #5239, #17980, #15643, #27841, #17008, #22128, #5353, #22358, #1182, #9692, #17977, #10649, #22101, #16384, #17663, #2604, #3097, #19199, #22098, #6521, #11884, #12088, #17797, #26005, #8310, #3205 ) ) ;
#25895 = EDGE_LOOP ( 'NONE', ( #1419, #19450, #1587, #12753 ) ) ;
#25896 = CARTESIAN_POINT ( 'NONE',  ( -0.3715251363271980245, 0.06498290224717540031, 0.1992125984251968684 ) ) ;
#25897 = EDGE_CURVE ( 'NONE', #22050, #3563, #5432, .T. ) ;
#25898 = CARTESIAN_POINT ( 'NONE',  ( 0.0002525749203916739381, 0.6881889763779529545, 0.3401599409343964431 ) ) ;
#25899 = DIRECTION ( 'NONE',  ( 1.000000000000000000, 0.000000000000000000, 0.000000000000000000 ) ) ;
#25900 = EDGE_CURVE ( 'NONE', #10034, #22689, #16187, .T. ) ;
#25901 = AXIS2_PLACEMENT_3D ( 'NONE', #6257, #10336, #8093 ) ;
#25902 = CARTESIAN_POINT ( 'NONE',  ( -0.4986013261500205074, 0.000000000000000000, -0.05856299212598425896 ) ) ;
#25903 = EDGE_CURVE ( 'NONE', #2742, #3153, #26285, .T. ) ;
#25904 = AXIS2_PLACEMENT_3D ( 'NONE', #26394, #3457, #16606 ) ;
#25905 = EDGE_LOOP ( 'NONE', ( #22133, #9375, #21014, #11952 ) ) ;
#25906 = CARTESIAN_POINT ( 'NONE',  ( 0.000000000000000000, 0.000000000000000000, 0.2574803149606298969 ) ) ;
#25907 = CARTESIAN_POINT ( 'NONE',  ( 0.000000000000000000, 0.000000000000000000, -0.1559029880880275776 ) ) ;
#25908 = CARTESIAN_POINT ( 'NONE',  ( -0.4921259842519395411, 0.03220957031763951872, -1.550196850393700920 ) ) ;
#25909 = EDGE_CURVE ( 'NONE', #3172, #9714, #11962, .T. ) ;
#25910 = CARTESIAN_POINT ( 'NONE',  ( -0.1458850421962728516, -0.4296318976990441407, -1.934055118110236338 ) ) ;
#25911 = EDGE_CURVE ( 'NONE', #10433, #2005, #14236, .T. ) ;
#25912 = TOROIDAL_SURFACE ( 'NONE', #13713, 0.5610236220472440971, 0.1003937007874015908 ) ;
#25913 = ( BOUNDED_CURVE ( )  B_SPLINE_CURVE ( 2, ( #1054, #18535, #7687 ),
 .UNSPECIFIED., .F., .T. ) 
 B_SPLINE_CURVE_WITH_KNOTS ( ( 3, 3 ),
 ( 0.000000000000000000, 0.2336872276155829986 ),
 .UNSPECIFIED. ) 
 CURVE ( )  GEOMETRIC_REPRESENTATION_ITEM ( )  RATIONAL_B_SPLINE_CURVE ( ( 1.000000000000000000, 1.154700538379243913, 1.000000000000000000 ) ) 
 REPRESENTATION_ITEM ( '' )  ) ;
#25914 = CARTESIAN_POINT ( 'NONE',  ( -0.6544535166833030937, -0.005594563712608583567, 0.07874015109845884652 ) ) ;
#25915 = DIRECTION ( 'NONE',  ( 0.000000000000000000, 1.000000000000000000, 0.000000000000000000 ) ) ;
#25916 = DIRECTION ( 'NONE',  ( 0.000000000000000000, 0.000000000000000000, 1.000000000000000000 ) ) ;
#25917 = VERTEX_POINT ( 'NONE', #12863 ) ;
#25918 = DIRECTION ( 'NONE',  ( -0.4999999999999998890, 0.8660254037844388186, 0.000000000000000000 ) ) ;
#25919 = CARTESIAN_POINT ( 'NONE',  ( 0.000000000000000000, 0.000000000000000000, 0.01181102362204724393 ) ) ;
#25920 = AXIS2_PLACEMENT_3D ( 'NONE', #20090, #9334, #26572 ) ;
#25921 = CARTESIAN_POINT ( 'NONE',  ( -0.3012109481301850633, 0.3598698725862389813, 0.1992125984251968684 ) ) ;
#25922 = CARTESIAN_POINT ( 'NONE',  ( -0.0001724821237274612798, 0.3771653543307086909, 0.1992150590373740204 ) ) ;
#25923 = ORIENTED_EDGE ( 'NONE', *, *, #3120, .F. ) ;
#25924 = CARTESIAN_POINT ( 'NONE',  ( -0.2991932138496531390, 0.3411003281196664516, -1.934055118110236338 ) ) ;
#25925 = LINE ( 'NONE', #26459, #4011 ) ;
#25926 = DIRECTION ( 'NONE',  ( 1.000000000000000000, 0.000000000000000000, 0.000000000000000000 ) ) ;
#25927 = CARTESIAN_POINT ( 'NONE',  ( 0.5526079293737076181, -0.1480156394741905801, 0.9399606299212598381 ) ) ;
#25928 = CARTESIAN_POINT ( 'NONE',  ( 0.3102399269716953345, -0.7316071111737637578, -0.6652804359117283628 ) ) ;
#25929 = CARTESIAN_POINT ( 'NONE',  ( 0.000000000000000000, 0.000000000000000000, 0.07637795275590551769 ) ) ;
#25930 = CIRCLE ( 'NONE', #15123, 0.1673228346456692994 ) ;
#25931 = EDGE_CURVE ( 'NONE', #22287, #4474, #14727, .T. ) ;
#25932 = CARTESIAN_POINT ( 'NONE',  ( 0.3350125228553208490, -0.2937477835499151535, -1.934055118110235894 ) ) ;
#25933 = CARTESIAN_POINT ( 'NONE',  ( 0.000000000000000000, 0.000000000000000000, 0.1377952755905511584 ) ) ;
#25934 = LINE ( 'NONE', #15078, #23807 ) ;
#25935 = CARTESIAN_POINT ( 'NONE',  ( -0.2230788859036007821, 0.2650812153444458419, 0.1377952755905510474 ) ) ;
#25936 = LINE ( 'NONE', #12381, #6323 ) ;
#25937 = EDGE_CURVE ( 'NONE', #1203, #15744, #8490, .T. ) ;
#25938 = ORIENTED_EDGE ( 'NONE', *, *, #3005, .T. ) ;
#25939 = CARTESIAN_POINT ( 'NONE',  ( -0.6117833106356003192, 0.1080972763116098551, 0.2574827755769819038 ) ) ;
#25940 = AXIS2_PLACEMENT_3D ( 'NONE', #17533, #4801, #6389 ) ;
#25941 = ORIENTED_EDGE ( 'NONE', *, *, #6680, .T. ) ;
#25942 = CARTESIAN_POINT ( 'NONE',  ( 0.000000000000000000, 0.000000000000000000, 0.1771653543307086520 ) ) ;
#25943 = ORIENTED_EDGE ( 'NONE', *, *, #7056, .F. ) ;
#25944 = ORIENTED_EDGE ( 'NONE', *, *, #23690, .T. ) ;
#25945 = PLANE ( 'NONE',  #23704 ) ;
#25946 = CARTESIAN_POINT ( 'NONE',  ( -0.1968503937007874127, 0.9448818897637796255, -1.639108661417322569E-17 ) ) ;
#25947 = SHAPE_DEFINITION_REPRESENTATION ( #18806, #19852 ) ;
#25948 = DIRECTION ( 'NONE',  ( 0.000000000000000000, 1.000000000000000000, 0.000000000000000000 ) ) ;
#25949 = VECTOR ( 'NONE', #19592, 39.37007874015748854 ) ;
#25950 = SURFACE_STYLE_USAGE ( .BOTH. , #9111 ) ;
#25951 = EDGE_CURVE ( 'NONE', #25584, #25182, #6134, .T. ) ;
#25952 = ORIENTED_EDGE ( 'NONE', *, *, #4307, .T. ) ;
#25953 = EDGE_LOOP ( 'NONE', ( #531, #26281 ) ) ;
#25954 = CARTESIAN_POINT ( 'NONE',  ( -0.3349073414798507953, 0.1651192144506273274, -3.115157480314960647 ) ) ;
#25955 = VERTEX_POINT ( 'NONE', #1989 ) ;
#25956 = CARTESIAN_POINT ( 'NONE',  ( 0.000000000000000000, 0.000000000000000000, -4.330708661417323135 ) ) ;
#25957 = ORIENTED_EDGE ( 'NONE', *, *, #18480, .F. ) ;
#25958 = B_SPLINE_CURVE_WITH_KNOTS ( 'NONE', 3,
 ( #24814, #11969, #14086, #22703, #25239, #5763 ),
 .UNSPECIFIED., .F., .F.,
 ( 4, 2, 4 ),
 ( 0.9359046326925629655, 0.9375808709372029925, 0.9392571091818440188 ),
 .UNSPECIFIED. ) ;
#25959 = DIRECTION ( 'NONE',  ( 0.000000000000000000, 1.000000000000000000, 0.000000000000000000 ) ) ;
#25960 = CARTESIAN_POINT ( 'NONE',  ( 0.04380447413658805633, -0.3324885138898231451, 1.953740157480315043 ) ) ;
#25961 = ORIENTED_EDGE ( 'NONE', *, *, #2158, .T. ) ;
#25962 = EDGE_LOOP ( 'NONE', ( #27561, #6992, #11913, #1005, #20914, #18361, #5578, #5746 ) ) ;
#25963 = CIRCLE ( 'NONE', #21841, 0.1299232283464566984 ) ;
#25964 = ORIENTED_EDGE ( 'NONE', *, *, #21081, .F. ) ;
#25965 = CARTESIAN_POINT ( 'NONE',  ( -4.821283464566928349E-18, 0.000000000000000000, -0.3779527559055118058 ) ) ;
#25966 = AXIS2_PLACEMENT_3D ( 'NONE', #21771, #13141, #23627 ) ;
#25967 = ORIENTED_EDGE ( 'NONE', *, *, #14363, .F. ) ;
#25968 = EDGE_LOOP ( 'NONE', ( #25861, #27501 ) ) ;
#25969 = ORIENTED_EDGE ( 'NONE', *, *, #20565, .T. ) ;
#25970 = FACE_OUTER_BOUND ( 'NONE', #9001, .T. ) ;
#25971 = EDGE_CURVE ( 'NONE', #9968, #26680, #23252, .T. ) ;
#25972 = CARTESIAN_POINT ( 'NONE',  ( -4.821283464566928349E-18, 0.000000000000000000, -0.02362204724409468909 ) ) ;
#25973 = CARTESIAN_POINT ( 'NONE',  ( -0.2979095355689177493, -0.6203660015065670663, 0.1322834645669291320 ) ) ;
#25974 = CARTESIAN_POINT ( 'NONE',  ( 0.7616545822564796397, 0.5977631770216751406, 0.08921608065419495137 ) ) ;
#25975 = ORIENTED_EDGE ( 'NONE', *, *, #26454, .F. ) ;
#25976 = EDGE_CURVE ( 'NONE', #18301, #26351, #25057, .T. ) ;
#25977 = AXIS2_PLACEMENT_3D ( 'NONE', #20238, #20661, #13738 ) ;
#25978 = FACE_BOUND ( 'NONE', #5765, .T. ) ;
#25979 = CARTESIAN_POINT ( 'NONE',  ( -0.3751294191746886164, 0.2999672986753446069, 0.2362204724409450174 ) ) ;
#25980 = DIRECTION ( 'NONE',  ( 0.000000000000000000, -7.180547322999998243E-06, -0.9999999999742198442 ) ) ;
#25981 = AXIS2_PLACEMENT_3D ( 'NONE', #11712, #20335, #18188 ) ;
#25982 = DIRECTION ( 'NONE',  ( 0.000000000000000000, 0.000000000000000000, -1.000000000000000000 ) ) ;
#25983 = DIRECTION ( 'NONE',  ( -1.000000000000000000, 0.000000000000000000, 0.000000000000000000 ) ) ;
#25984 = EDGE_CURVE ( 'NONE', #5951, #9013, #2308, .T. ) ;
#25985 = CIRCLE ( 'NONE', #17409, 0.4786070381542913421 ) ;
#25986 = CARTESIAN_POINT ( 'NONE',  ( -0.07870736599817813872, 0.2165354330708661457, -3.212150913008700481 ) ) ;
#25987 = VERTEX_POINT ( 'NONE', #5860 ) ;
#25988 = CARTESIAN_POINT ( 'NONE',  ( 0.4157391792961063204, 0.3323952789219082882, 0.1322834645669291320 ) ) ;
#25989 = ORIENTED_EDGE ( 'NONE', *, *, #23764, .T. ) ;
#25990 = LINE ( 'NONE', #6920, #17107 ) ;
#25991 = ORIENTED_EDGE ( 'NONE', *, *, #25971, .T. ) ;
#25992 = FACE_OUTER_BOUND ( 'NONE', #14887, .T. ) ;
#25993 = CARTESIAN_POINT ( 'NONE',  ( 0.000000000000000000, 0.6102362204724409711, 0.2362204724409449064 ) ) ;
#25994 = CARTESIAN_POINT ( 'NONE',  ( 0.3334645669291338987, -0.8041772776331653771, -0.9118913923173522784 ) ) ;
#25995 = EDGE_LOOP ( 'NONE', ( #25882, #25080 ) ) ;
#25996 = CARTESIAN_POINT ( 'NONE',  ( -0.4152525734086685016, 0.3642352168757148623, 0.9399606299212598381 ) ) ;
#25997 = CARTESIAN_POINT ( 'NONE',  ( 0.000000000000000000, 0.000000000000000000, -2.322834645648385710 ) ) ;
#25998 = ORIENTED_EDGE ( 'NONE', *, *, #14761, .T. ) ;
#25999 = CARTESIAN_POINT ( 'NONE',  ( 0.2362204724225640262, 0.000000000000000000, -3.149606299191693548 ) ) ;
#26000 = SURFACE_STYLE_FILL_AREA ( #12719 ) ;
#26001 = AXIS2_PLACEMENT_3D ( 'NONE', #23341, #3967, #53 ) ;
#26002 = FACE_OUTER_BOUND ( 'NONE', #2420, .T. ) ;
#26003 = DIRECTION ( 'NONE',  ( 0.000000000000000000, -1.000000000000000000, 0.000000000000000000 ) ) ;
#26004 = CARTESIAN_POINT ( 'NONE',  ( 0.09842519685039351207, 0.1968503937007873850, -3.548228346456693050 ) ) ;
#26005 = ADVANCED_FACE ( 'NONE', ( #25730 ), #22950, .T. ) ;
#26006 = VECTOR ( 'NONE', #3135, 39.37007874015748143 ) ;
#26007 = EDGE_CURVE ( 'NONE', #5696, #20978, #9939, .T. ) ;
#26008 = CARTESIAN_POINT ( 'NONE',  ( -0.0005189969344232283309, 0.3771649972486724733, 0.1992125984251968684 ) ) ;
#26009 = DIRECTION ( 'NONE',  ( -1.000000000000000000, 0.000000000000000000, 0.000000000000000000 ) ) ;
#26010 = CARTESIAN_POINT ( 'NONE',  ( -0.2420394123212937232, 0.2892587550802429575, 0.07637795275590551769 ) ) ;
#26011 = DIRECTION ( 'NONE',  ( -0.8660254037844385966, 0.4999999999999998335, 0.000000000000000000 ) ) ;
#26012 = FACE_OUTER_BOUND ( 'NONE', #4163, .T. ) ;
#26013 = DIRECTION ( 'NONE',  ( 0.000000000000000000, 1.000000000000000000, 0.000000000000000000 ) ) ;
#26014 = CARTESIAN_POINT ( 'NONE',  ( 0.5708661417322835607, 0.03736310157557569400, 0.9399606299212598381 ) ) ;
#26015 = CARTESIAN_POINT ( 'NONE',  ( 0.0006679551606482677165, 0.5322830454629158270, 0.3401574803149606252 ) ) ;
#26016 = ORIENTED_EDGE ( 'NONE', *, *, #7300, .F. ) ;
#26017 = CARTESIAN_POINT ( 'NONE',  ( 0.000000000000000000, 0.000000000000000000, 0.2574803149606298969 ) ) ;
#26018 = AXIS2_PLACEMENT_3D ( 'NONE', #3653, #16516, #27687 ) ;
#26019 = EDGE_LOOP ( 'NONE', ( #16698, #16247, #25806, #5283 ) ) ;
#26020 = CIRCLE ( 'NONE', #771, 0.01181102362204755271 ) ;
#26021 = ORIENTED_EDGE ( 'NONE', *, *, #4475, .F. ) ;
#26022 = EDGE_CURVE ( 'NONE', #23891, #18882, #9717, .T. ) ;
#26023 = CIRCLE ( 'NONE', #14296, 0.5905511811023621549 ) ;
#26024 = B_SPLINE_CURVE_WITH_KNOTS ( 'NONE', 2,
 ( #9993, #20871, #5485 ),
 .UNSPECIFIED., .F., .F.,
 ( 3, 3 ),
 ( 0.000000000000000000, 1.000000000000000000 ),
 .UNSPECIFIED. ) ;
#26025 = DIRECTION ( 'NONE',  ( 0.000000000000000000, 0.000000000000000000, 1.000000000000000000 ) ) ;
#26026 = CARTESIAN_POINT ( 'NONE',  ( -0.1771653543307086520, 0.000000000000000000, 0.000000000000000000 ) ) ;
#26027 = CARTESIAN_POINT ( 'NONE',  ( 0.4834654033849994370, -0.1110087727130258245, 0.1734435147525180132 ) ) ;
#26028 = LINE ( 'NONE', #15171, #11866 ) ;
#26029 = ORIENTED_EDGE ( 'NONE', *, *, #4798, .F. ) ;
#26030 = LINE ( 'NONE', #24042, #27781 ) ;
#26031 = ORIENTED_EDGE ( 'NONE', *, *, #1526, .T. ) ;
#26032 = CARTESIAN_POINT ( 'NONE',  ( 0.000000000000000000, 0.000000000000000000, 0.1771653543307086520 ) ) ;
#26033 = CARTESIAN_POINT ( 'NONE',  ( -0.4537304931026616139, 0.07942646906834205378, 0.1771653543307086243 ) ) ;
#26034 = CARTESIAN_POINT ( 'NONE',  ( -0.3990005999895763766, 0.4761957181734953193, 0.2574819594177531479 ) ) ;
#26035 = CARTESIAN_POINT ( 'NONE',  ( -0.0005189969344232283309, 0.3771649972486724733, 0.07637795275590551769 ) ) ;
#26036 = CARTESIAN_POINT ( 'NONE',  ( 0.1694923354752467248, -0.4674199084428152240, 0.1140743250954091431 ) ) ;
#26037 = CARTESIAN_POINT ( 'NONE',  ( 0.2983664441503059428, -0.6201464311010157493, 0.1322810039474933141 ) ) ;
#26038 = AXIS2_PLACEMENT_3D ( 'NONE', #6511, #15143, #12996 ) ;
#26039 = ORIENTED_EDGE ( 'NONE', *, *, #27146, .F. ) ;
#26040 = DIRECTION ( 'NONE',  ( 0.000000000000000000, 0.000000000000000000, -1.000000000000000000 ) ) ;
#26041 = CARTESIAN_POINT ( 'NONE',  ( -0.4423390553432706152, 0.2180862235769438773, -1.550196850393700920 ) ) ;
#26042 = CARTESIAN_POINT ( 'NONE',  ( 0.1188866373884749916, -0.4438564651657395665, -1.928289503579163178 ) ) ;
#26043 = DIRECTION ( 'NONE',  ( -0.000000000000000000, -0.000000000000000000, 1.000000000000000000 ) ) ;
#26044 = CARTESIAN_POINT ( 'NONE',  ( -0.6434710025615986151, -0.04048505764336882140, 0.07811204921870905371 ) ) ;
#26045 = CARTESIAN_POINT ( 'NONE',  ( 0.4777261797697372470, -0.2355331214654103889, 1.747047244094488194 ) ) ;
#26046 = FACE_OUTER_BOUND ( 'NONE', #9954, .T. ) ;
#26047 = ORIENTED_EDGE ( 'NONE', *, *, #10426, .T. ) ;
#26048 = AXIS2_PLACEMENT_3D ( 'NONE', #25012, #12156, #18645 ) ;
#26049 = CARTESIAN_POINT ( 'NONE',  ( -0.6299212598425196763, 0.000000000000000000, 0.000000000000000000 ) ) ;
#26050 = CARTESIAN_POINT ( 'NONE',  ( -0.6212843287616266474, -0.6280845039693049303, 0.9045795100263914756 ) ) ;
#26051 = B_SPLINE_CURVE_WITH_KNOTS ( 'NONE', 3,
 ( #14627, #4140, #14903, #16865 ),
 .UNSPECIFIED., .F., .F.,
 ( 4, 4 ),
 ( 0.3864984308775630262, 0.3881911340211371408 ),
 .UNSPECIFIED. ) ;
#26052 = CARTESIAN_POINT ( 'NONE',  ( 0.000000000000000000, 0.000000000000000000, 0.3401574803149606252 ) ) ;
#26053 = AXIS2_PLACEMENT_3D ( 'NONE', #17180, #25795, #6443 ) ;
#26054 = ORIENTED_EDGE ( 'NONE', *, *, #4377, .T. ) ;
#26055 = FACE_OUTER_BOUND ( 'NONE', #1775, .T. ) ;
#26056 = EDGE_CURVE ( 'NONE', #19645, #1011, #6617, .T. ) ;
#26057 = DIRECTION ( 'NONE',  ( 0.000000000000000000, 1.000000000000000000, 0.000000000000000000 ) ) ;
#26058 = CARTESIAN_POINT ( 'NONE',  ( 0.3543307086614173596, -0.02319089060379044345, 1.953740157480315043 ) ) ;
#26059 = ORIENTED_EDGE ( 'NONE', *, *, #10547, .F. ) ;
#26060 = CIRCLE ( 'NONE', #17490, 0.8031496062992127261 ) ;
#26061 = DIRECTION ( 'NONE',  ( 7.017815000000000124E-18, -1.000000000000000000, 0.000000000000000000 ) ) ;
#26062 = DIRECTION ( 'NONE',  ( 0.000000000000000000, 0.000000000000000000, 1.000000000000000000 ) ) ;
#26063 = FACE_OUTER_BOUND ( 'NONE', #24273, .T. ) ;
#26064 = ADVANCED_FACE ( 'NONE', ( #8765 ), #7974, .T. ) ;
#26065 = ( REPRESENTATION_RELATIONSHIP ('NONE','NONE', #12434, #3575 ) REPRESENTATION_RELATIONSHIP_WITH_TRANSFORMATION ( #7194 )SHAPE_REPRESENTATION_RELATIONSHIP( ) ) ;
#26066 = FACE_OUTER_BOUND ( 'NONE', #27358, .T. ) ;
#26067 = CARTESIAN_POINT ( 'NONE',  ( -0.05811937031499277845, -0.4417502570510357662, -1.934055118110236338 ) ) ;
#26068 = CARTESIAN_POINT ( 'NONE',  ( -0.09660931395005439848, 0.3606853515406323596, -3.115157480314960647 ) ) ;
#26069 = ( CONVERSION_BASED_UNIT ( 'INCH', #26201 ) LENGTH_UNIT ( ) NAMED_UNIT ( #18919 ) ) ;
#26070 = CARTESIAN_POINT ( 'NONE',  ( 4.821444091131312140E-17, 0.03937007874015747977, 0.3937007874015748254 ) ) ;
#26071 = DIRECTION ( 'NONE',  ( 0.000000000000000000, 0.000000000000000000, 1.000000000000000000 ) ) ;
#26072 = CIRCLE ( 'NONE', #13885, 0.3937007874015748254 ) ;
#26073 = EDGE_LOOP ( 'NONE', ( #20932, #13792, #25123, #13823, #16867, #5406, #1915, #7890, #22542, #11560 ) ) ;
#26074 = CARTESIAN_POINT ( 'NONE',  ( -0.4446020952038907681, 0.000000000000000000, -1.934055118110236338 ) ) ;
#26075 = CIRCLE ( 'NONE', #2610, 0.1771653543307086520 ) ;
#26076 = EDGE_LOOP ( 'NONE', ( #151, #11321, #12781, #25320 ) ) ;
#26077 = ORIENTED_EDGE ( 'NONE', *, *, #9288, .T. ) ;
#26078 = CARTESIAN_POINT ( 'NONE',  ( 0.4716287720757130764, -0.1069935333116923404, 0.2715646632655941972 ) ) ;
#26079 = APPLICATION_PROTOCOL_DEFINITION ( 'draft international standard', 'automotive_design', 1998, #9805 ) ;
#26080 = CARTESIAN_POINT ( 'NONE',  ( -0.5118110236220472231, -0.03349795313264326835, 1.766732283464566899 ) ) ;
#26081 = CARTESIAN_POINT ( 'NONE',  ( -0.4600326175560697783, 0.2268096725222554233, 1.747047244094488194 ) ) ;
#26082 = CYLINDRICAL_SURFACE ( 'NONE', #23984, 0.1181102362204720091 ) ;
#26083 = VERTEX_POINT ( 'NONE', #2263 ) ;
#26084 = EDGE_CURVE ( 'NONE', #24622, #20206, #3364, .T. ) ;
#26085 = ORIENTED_EDGE ( 'NONE', *, *, #24120, .F. ) ;
#26086 = CARTESIAN_POINT ( 'NONE',  ( 0.09660931395005455113, -0.3606853515406215904, -3.115157480314960647 ) ) ;
#26087 = ORIENTED_EDGE ( 'NONE', *, *, #22177, .F. ) ;
#26088 = ORIENTED_EDGE ( 'NONE', *, *, #2298, .T. ) ;
#26089 = CARTESIAN_POINT ( 'NONE',  ( 0.1120675189988346587, -0.4694218845611126678, -0.3846748511993476338 ) ) ;
#26090 = ( NAMED_UNIT ( * ) SI_UNIT ( $, .STERADIAN. ) SOLID_ANGLE_UNIT ( ) ) ;
#26091 = CARTESIAN_POINT ( 'NONE',  ( 0.1493967478962657525, 0.2562458715718933799, -0.4061682508616698550 ) ) ;
#26092 = ADVANCED_FACE ( 'NONE', ( #23757, #16577 ), #15559, .T. ) ;
#26093 = AXIS2_PLACEMENT_3D ( 'NONE', #15784, #5037, #4899 ) ;
#26094 = CARTESIAN_POINT ( 'NONE',  ( -0.3239425792934414461, 0.08676778863010937981, 1.953740157480315043 ) ) ;
#26095 = ORIENTED_EDGE ( 'NONE', *, *, #1911, .F. ) ;
#26096 = VERTEX_POINT ( 'NONE', #197 ) ;
#26097 = CARTESIAN_POINT ( 'NONE',  ( 0.4585215200179055817, -2.840735999735804609E-17, -1.928289503579156516 ) ) ;
#26098 = EDGE_CURVE ( 'NONE', #11701, #21231, #23274, .T. ) ;
#26099 = CIRCLE ( 'NONE', #13916, 0.4173606904906118076 ) ;
#26100 = VERTEX_POINT ( 'NONE', #21770 ) ;
#26101 = ORIENTED_EDGE ( 'NONE', *, *, #19019, .T. ) ;
#26102 = ORIENTED_EDGE ( 'NONE', *, *, #15491, .T. ) ;
#26103 = DIRECTION ( 'NONE',  ( 0.000000000000000000, 0.000000000000000000, 1.000000000000000000 ) ) ;
#26104 = CARTESIAN_POINT ( 'NONE',  ( 0.4986013261500205074, 6.106105181202481056E-17, -0.05856299212598425896 ) ) ;
#26105 = CARTESIAN_POINT ( 'NONE',  ( 0.000000000000000000, 0.000000000000000000, -4.291338582656260670 ) ) ;
#26106 = VECTOR ( 'NONE', #19936, 39.37007874015748143 ) ;
#26107 = CARTESIAN_POINT ( 'NONE',  ( 0.6427545578076259147, 0.8597063426663432706, -0.09226840441818499883 ) ) ;
#26108 = EDGE_CURVE ( 'NONE', #16453, #18664, #16477, .T. ) ;
#26109 = EDGE_LOOP ( 'NONE', ( #15309, #11257, #12512, #4062 ) ) ;
#26110 = DIRECTION ( 'NONE',  ( 0.6698894744055998718, -8.203780006133206145E-17, 0.7424608353849979636 ) ) ;
#26111 = AXIS2_PLACEMENT_3D ( 'NONE', #17179, #2829, #26431 ) ;
#26112 = CARTESIAN_POINT ( 'NONE',  ( -0.5188885761056504231, -0.1186607836835326668, 0.3401599409343964431 ) ) ;
#26113 = CARTESIAN_POINT ( 'NONE',  ( -0.3617579313041923705, -1.110209215450335796, -0.3979864608631387690 ) ) ;
#26114 = CIRCLE ( 'NONE', #4459, 0.2952755905511805223 ) ;
#26115 = CIRCLE ( 'NONE', #5366, 0.4606299212598425341 ) ;
#26116 = DIRECTION ( 'NONE',  ( 1.000000000000000000, 0.000000000000000000, 0.000000000000000000 ) ) ;
#26117 = DIRECTION ( 'NONE',  ( -1.000000000000000000, 1.224646799147353454E-16, 0.000000000000000000 ) ) ;
#26118 = FACE_BOUND ( 'NONE', #6539, .T. ) ;
#26119 = EDGE_CURVE ( 'NONE', #14713, #12635, #20080, .T. ) ;
#26120 = CARTESIAN_POINT ( 'NONE',  ( -0.04956879678463866484, 0.1968503937007873850, -3.186635197791150453 ) ) ;
#26121 = EDGE_LOOP ( 'NONE', ( #10477, #9682, #15716, #881, #19610, #11140 ) ) ;
#26122 = CIRCLE ( 'NONE', #10778, 0.07910393700787400617 ) ;
#26123 = CARTESIAN_POINT ( 'NONE',  ( -0.05118110236220472370, 0.000000000000000000, 0.000000000000000000 ) ) ;
#26124 = EDGE_CURVE ( 'NONE', #14972, #7615, #26404, .T. ) ;
#26125 = ORIENTED_EDGE ( 'NONE', *, *, #21299, .T. ) ;
#26126 = DIRECTION ( 'NONE',  ( 1.000000000000000000, 0.000000000000000000, 0.000000000000000000 ) ) ;
#26127 = ( BOUNDED_CURVE ( )  B_SPLINE_CURVE ( 2, ( #16427, #14468, #25609 ),
 .UNSPECIFIED., .F., .F. ) 
 B_SPLINE_CURVE_WITH_KNOTS ( ( 3, 3 ),
 ( 0.000000000000000000, 0.5842180690389588982 ),
 .UNSPECIFIED. ) 
 CURVE ( )  GEOMETRIC_REPRESENTATION_ITEM ( )  RATIONAL_B_SPLINE_CURVE ( ( 1.000000000000000000, 1.154700538379251906, 1.000000000000000000 ) ) 
 REPRESENTATION_ITEM ( '' )  ) ;
#26128 = CARTESIAN_POINT ( 'NONE',  ( -0.1589886963207482462, -0.4351482077919938685, 0.1494804571204739196 ) ) ;
#26129 = CARTESIAN_POINT ( 'NONE',  ( 0.7168072604729537334, -0.1644124225521826632, 0.1960773254416929845 ) ) ;
#26130 = CARTESIAN_POINT ( 'NONE',  ( 0.7165354330708662012, 0.000000000000000000, 0.3543307086614173040 ) ) ;
#26131 = ORIENTED_EDGE ( 'NONE', *, *, #25526, .T. ) ;
#26132 = CARTESIAN_POINT ( 'NONE',  ( 0.5230301363771271417, 0.1775991818008589573, 0.9399606299212598381 ) ) ;
#26133 = DIRECTION ( 'NONE',  ( 0.000000000000000000, 0.000000000000000000, -1.000000000000000000 ) ) ;
#26134 = EDGE_CURVE ( 'NONE', #8508, #17093, #22225, .T. ) ;
#26135 = CARTESIAN_POINT ( 'NONE',  ( -0.6562077975700453258, 2.612916929133858441E-14, 0.2362204724409449064 ) ) ;
#26136 = ORIENTED_EDGE ( 'NONE', *, *, #25029, .F. ) ;
#26137 = CIRCLE ( 'NONE', #21628, 0.4456396174367268093 ) ;
#26138 = DIRECTION ( 'NONE',  ( 1.000000000000000000, 0.000000000000000000, -0.000000000000000000 ) ) ;
#26139 = CARTESIAN_POINT ( 'NONE',  ( 0.4165721057576322606, 0.3313508221749649763, 0.1322834645669291320 ) ) ;
#26140 = DIRECTION ( 'NONE',  ( 0.000000000000000000, 0.000000000000000000, 1.000000000000000000 ) ) ;
#26141 = B_SPLINE_CURVE_WITH_KNOTS ( 'NONE', 3,
 ( #27020, #20092, #15850, #19956, #610, #15722 ),
 .UNSPECIFIED., .F., .F.,
 ( 4, 2, 4 ),
 ( 0.5000000000000000000, 0.7500000000000000000, 1.000000000000000000 ),
 .UNSPECIFIED. ) ;
#26142 = CARTESIAN_POINT ( 'NONE',  ( 0.4167985568850881561, 0.07349283109919291235, 0.1377952755905511861 ) ) ;
#26143 = DIRECTION ( 'NONE',  ( 0.000000000000000000, 1.000000000000000000, 0.000000000000000000 ) ) ;
#26144 = CARTESIAN_POINT ( 'NONE',  ( 0.4897507849329837404, 0.08575075074624730065, 0.1615162260786077997 ) ) ;
#26145 = DIRECTION ( 'NONE',  ( -0.9790454724845842893, -0.1018208755700882318, 0.1763589297585410332 ) ) ;
#26146 = DIRECTION ( 'NONE',  ( 0.000000000000000000, 0.000000000000000000, 1.000000000000000000 ) ) ;
#26147 = ORIENTED_EDGE ( 'NONE', *, *, #4258, .T. ) ;
#26148 = FACE_OUTER_BOUND ( 'NONE', #9870, .T. ) ;
#26149 = CARTESIAN_POINT ( 'NONE',  ( 0.5671862884095085766, -0.07472527936312026164, 0.9399606299212598381 ) ) ;
#26150 = CARTESIAN_POINT ( 'NONE',  ( 0.6140435224042697371, 0.000000000000000000, 0.000000000000000000 ) ) ;
#26151 = VERTEX_POINT ( 'NONE', #6938 ) ;
#26152 = CARTESIAN_POINT ( 'NONE',  ( -0.5099673189338885804, -0.1157175986333887352, 0.3331434174569700146 ) ) ;
#26153 = AXIS2_PLACEMENT_3D ( 'NONE', #18032, #26674, #22032 ) ;
#26154 = VERTEX_POINT ( 'NONE', #19918 ) ;
#26155 = CARTESIAN_POINT ( 'NONE',  ( 0.000000000000000000, 0.000000000000000000, 0.4724409448818898127 ) ) ;
#26156 = EDGE_CURVE ( 'NONE', #3371, #21006, #21891, .T. ) ;
#26157 = ORIENTED_EDGE ( 'NONE', *, *, #8694, .F. ) ;
#26158 = ADVANCED_FACE ( 'NONE', ( #24288 ), #26271, .T. ) ;
#26159 = CARTESIAN_POINT ( 'NONE',  ( -0.09139240964747710749, -0.07874015748031500117, -1.188614124534770567E-17 ) ) ;
#26160 = CARTESIAN_POINT ( 'NONE',  ( 0.000000000000000000, 0.000000000000000000, 0.4062992125984251635 ) ) ;
#26161 = FACE_BOUND ( 'NONE', #3459, .T. ) ;
#26162 = CARTESIAN_POINT ( 'NONE',  ( 0.3713448905834433322, 0.06600512665679410251, 0.07637795275590551769 ) ) ;
#26163 = ORIENTED_EDGE ( 'NONE', *, *, #232, .F. ) ;
#26164 = DIRECTION ( 'NONE',  ( 0.000000000000000000, 0.000000000000000000, -1.000000000000000000 ) ) ;
#26165 = ORIENTED_EDGE ( 'NONE', *, *, #21415, .T. ) ;
#26166 = DIRECTION ( 'NONE',  ( -0.000000000000000000, -1.000000000000000000, -0.000000000000000000 ) ) ;
#26167 = DIRECTION ( 'NONE',  ( -0.8660254037844382635, -0.5000000000000005551, 0.000000000000000000 ) ) ;
#26168 = CIRCLE ( 'NONE', #14456, 0.1771653543307086798 ) ;
#26169 = CARTESIAN_POINT ( 'NONE',  ( 0.3771653543307086909, 0.000000000000000000, 0.1992125984251968684 ) ) ;
#26170 = B_SPLINE_CURVE_WITH_KNOTS ( 'NONE', 3,
 ( #26887, #7537, #27182, #24904, #17962, #26600, #22793, #9930, #16019, #15746 ),
 .UNSPECIFIED., .F., .F.,
 ( 4, 2, 2, 2, 4 ),
 ( 0.000000000000000000, 0.2499999999999998335, 0.4999999999999996669, 0.7499999999999997780, 1.000000000000000000 ),
 .UNSPECIFIED. ) ;
#26171 = CIRCLE ( 'NONE', #23926, 0.5531496062992126150 ) ;
#26172 = DIRECTION ( 'NONE',  ( 0.000000000000000000, 1.000000000000000000, 0.000000000000000000 ) ) ;
#26173 = B_SPLINE_CURVE_WITH_KNOTS ( 'NONE', 3,
 ( #26450, #21684, #11350, #19967, #24338, #7113, #17573, #13185, #15736, #2311 ),
 .UNSPECIFIED., .F., .F.,
 ( 4, 2, 2, 2, 4 ),
 ( 0.000000000000000000, 0.2500000000000000000, 0.5000000000000000000, 0.7500000000000000000, 1.000000000000000000 ),
 .UNSPECIFIED. ) ;
#26174 = DIRECTION ( 'NONE',  ( 1.224646799147353207E-16, 1.000000000000000000, -0.000000000000000000 ) ) ;
#26175 = EDGE_LOOP ( 'NONE', ( #24000, #25197, #12811, #14303, #21173, #2659 ) ) ;
#26176 = CARTESIAN_POINT ( 'NONE',  ( -4.618943439303797186E-17, -0.3771653543307086909, 0.2374015748031496065 ) ) ;
#26177 = CARTESIAN_POINT ( 'NONE',  ( -0.3252100150720236282, -0.3707612262533184766, -1.569881889763779625 ) ) ;
#26178 = CARTESIAN_POINT ( 'NONE',  ( 0.3645739570812633890, 0.2796934465393874358, -1.928289503579156072 ) ) ;
#26179 = VERTEX_POINT ( 'NONE', #2399 ) ;
#26180 = CARTESIAN_POINT ( 'NONE',  ( 0.2297883689023240139, -0.3979194638820313656, -1.928289503579174280 ) ) ;
#26181 = FACE_OUTER_BOUND ( 'NONE', #17775, .T. ) ;
#26182 = ADVANCED_BREP_SHAPE_REPRESENTATION ( 'Shaft Seal 15x26x7', ( #22141, #11588 ), #6215 ) ;
#26183 = CARTESIAN_POINT ( 'NONE',  ( 0.000000000000000000, 0.6212598425196850238, 0.3543307086614173040 ) ) ;
#26184 = CARTESIAN_POINT ( 'NONE',  ( -0.6305589872448129629, -0.08116040399610512102, 0.07586106382108366575 ) ) ;
#26185 = CARTESIAN_POINT ( 'NONE',  ( 0.000000000000000000, 0.000000000000000000, 0.07637795275590551769 ) ) ;
#26186 = EDGE_CURVE ( 'NONE', #17148, #14935, #6038, .T. ) ;
#26187 = FACE_OUTER_BOUND ( 'NONE', #1534, .T. ) ;
#26188 = CARTESIAN_POINT ( 'NONE',  ( -0.1707210962531915677, -0.4707890492249701131, 0.2574803149606298969 ) ) ;
#26189 = ORIENTED_EDGE ( 'NONE', *, *, #6680, .F. ) ;
#26190 = CARTESIAN_POINT ( 'NONE',  ( 0.3990005999895235855, 0.4761957181735393396, 0.2574819594177527593 ) ) ;
#26191 = DIRECTION ( 'NONE',  ( -0.7071067818211409506, 0.7071067805519539728, 8.659560554583403090E-17 ) ) ;
#26192 = CARTESIAN_POINT ( 'NONE',  ( -0.7635713814939685262, 0.3957398197978322374, 0.1751423728567907401 ) ) ;
#26193 = ORIENTED_EDGE ( 'NONE', *, *, #862, .T. ) ;
#26194 = CARTESIAN_POINT ( 'NONE',  ( -0.4527559054764770385, 0.000000000000000000, -1.934055118110236338 ) ) ;
#26195 = VECTOR ( 'NONE', #22285, 39.37007874015748854 ) ;
#26196 = CARTESIAN_POINT ( 'NONE',  ( 0.1490609433615242285, 0.000000000000000000, 0.000000000000000000 ) ) ;
#26197 = CARTESIAN_POINT ( 'NONE',  ( -0.3334645669291338987, 1.286842404713327115, -0.9809137335991812146 ) ) ;
#26198 = DIRECTION ( 'NONE',  ( 0.000000000000000000, 1.000000000000000000, -1.224646799147353207E-16 ) ) ;
#26199 = DIRECTION ( 'NONE',  ( 0.000000000000000000, -1.000000000000000000, 0.000000000000000000 ) ) ;
#26200 = CARTESIAN_POINT ( 'NONE',  ( 0.1651192144506298254, 0.3349073414798210413, -3.115157480314960647 ) ) ;
#26201 = LENGTH_MEASURE_WITH_UNIT ( LENGTH_MEASURE( 0.02539999999999999897 ), #2328 ) ;
#26202 = DIRECTION ( 'NONE',  ( 0.000000000000000000, 0.000000000000000000, -1.000000000000000000 ) ) ;
#26203 = CARTESIAN_POINT ( 'NONE',  ( -0.01968503937007873988, 0.000000000000000000, 0.000000000000000000 ) ) ;
#26204 = ADVANCED_FACE ( 'NONE', ( #17652 ), #22816, .T. ) ;
#26205 = ORIENTED_EDGE ( 'NONE', *, *, #25273, .F. ) ;
#26206 = EDGE_CURVE ( 'NONE', #12846, #8161, #12883, .T. ) ;
#26207 = CARTESIAN_POINT ( 'NONE',  ( -0.1288129352161812846, -0.4793172621399191535, -1.569881889763779848 ) ) ;
#26208 = VECTOR ( 'NONE', #11219, 39.37007874015748143 ) ;
#26209 = CIRCLE ( 'NONE', #9978, 0.6881889763779527325 ) ;
#26210 = ORIENTED_EDGE ( 'NONE', *, *, #27426, .T. ) ;
#26211 = EDGE_CURVE ( 'NONE', #7455, #21621, #15494, .T. ) ;
#26212 = EDGE_CURVE ( 'NONE', #7459, #247, #13690, .T. ) ;
#26213 = ORIENTED_EDGE ( 'NONE', *, *, #24508, .F. ) ;
#26214 = CARTESIAN_POINT ( 'NONE',  ( -0.1968503937007874127, -1.381459842519685169E-18, 0.09092130223458683158 ) ) ;
#26215 = APPLICATION_PROTOCOL_DEFINITION ( 'draft international standard', 'automotive_design', 1998, #21371 ) ;
#26216 = CARTESIAN_POINT ( 'NONE',  ( 0.000000000000000000, 0.000000000000000000, -3.278217716535432842E-17 ) ) ;
#26217 = DIRECTION ( 'NONE',  ( 0.000000000000000000, 0.000000000000000000, 1.000000000000000000 ) ) ;
#26218 = ORIENTED_EDGE ( 'NONE', *, *, #24206, .T. ) ;
#26219 = ORIENTED_EDGE ( 'NONE', *, *, #25748, .F. ) ;
#26220 = CARTESIAN_POINT ( 'NONE',  ( 0.1651192144506304360, -0.3349073414798397486, -3.115157480314960647 ) ) ;
#26221 = CARTESIAN_POINT ( 'NONE',  ( 0.2428345617565153547, 0.2885915454824177218, 0.07637795275590551769 ) ) ;
#26222 = ( REPRESENTATION_RELATIONSHIP ('NONE','NONE', #12434, #6338 ) REPRESENTATION_RELATIONSHIP_WITH_TRANSFORMATION ( #20754 )SHAPE_REPRESENTATION_RELATIONSHIP( ) ) ;
#26223 = ORIENTED_EDGE ( 'NONE', *, *, #1134, .T. ) ;
#26224 = CARTESIAN_POINT ( 'NONE',  ( -0.5375739373539409893, 0.4296723508511047229, 0.3401574803149606252 ) ) ;
#26225 = CYLINDRICAL_SURFACE ( 'NONE', #15025, 0.6299212598425196763 ) ;
#26226 = CARTESIAN_POINT ( 'NONE',  ( 0.1078280746903870629, -0.3175540113612215221, 1.953740157480315043 ) ) ;
#26227 = VERTEX_POINT ( 'NONE', #11027 ) ;
#26228 = VERTEX_POINT ( 'NONE', #26532 ) ;
#26229 = AXIS2_PLACEMENT_3D ( 'NONE', #22799, #21246, #19113 ) ;
#26230 = CARTESIAN_POINT ( 'NONE',  ( -0.07874015748031489015, 0.000000000000000000, -0.2834645669291338543 ) ) ;
#26231 = ORIENTED_EDGE ( 'NONE', *, *, #13343, .T. ) ;
#26232 = ORIENTED_EDGE ( 'NONE', *, *, #11935, .T. ) ;
#26233 = ORIENTED_EDGE ( 'NONE', *, *, #267, .F. ) ;
#26234 = DIRECTION ( 'NONE',  ( -0.9396926207859083169, 0.3420201433256692125, 0.000000000000000000 ) ) ;
#26235 = AXIS2_PLACEMENT_3D ( 'NONE', #14594, #1705, #14877 ) ;
#26236 = AXIS2_PLACEMENT_3D ( 'NONE', #27623, #10092, #7989 ) ;
#26237 = EDGE_CURVE ( 'NONE', #4219, #6332, #14745, .T. ) ;
#26238 = DIRECTION ( 'NONE',  ( 0.000000000000000000, 1.000000000000000000, 0.000000000000000000 ) ) ;
#26239 = CARTESIAN_POINT ( 'NONE',  ( 0.09590060490395689585, -0.2273032555864669124, 2.185478346456692557E-17 ) ) ;
#26240 = CARTESIAN_POINT ( 'NONE',  ( 0.5994540303786097812, 0.9188646166935047210, -0.1488510697577987707 ) ) ;
#26241 = EDGE_LOOP ( 'NONE', ( #10282, #4033 ) ) ;
#26242 = EDGE_CURVE ( 'NONE', #21440, #10683, #16105, .T. ) ;
#26243 = DIRECTION ( 'NONE',  ( 0.000000000000000000, 0.000000000000000000, -1.000000000000000000 ) ) ;
#26244 = EDGE_CURVE ( 'NONE', #21106, #6811, #16972, .T. ) ;
#26245 = EDGE_CURVE ( 'NONE', #3330, #14826, #10170, .T. ) ;
#26246 = CARTESIAN_POINT ( 'NONE',  ( 0.1109424284362303254, 0.000000000000000000, 0.000000000000000000 ) ) ;
#26247 = AXIS2_PLACEMENT_3D ( 'NONE', #27150, #1297, #21061 ) ;
#26248 = DIRECTION ( 'NONE',  ( 0.000000000000000000, 0.000000000000000000, -1.000000000000000000 ) ) ;
#26249 = EDGE_CURVE ( 'NONE', #14009, #3213, #3877, .T. ) ;
#26250 = CARTESIAN_POINT ( 'NONE',  ( 0.07874015748031495954, 0.005900511533401469472, -0.4653540093967190039 ) ) ;
#26251 = CARTESIAN_POINT ( 'NONE',  ( 0.000000000000000000, 0.000000000000000000, 1.953740157480315043 ) ) ;
#26252 = CARTESIAN_POINT ( 'NONE',  ( 0.4954415918530860607, 0.1327036767659604266, 1.766732283464566899 ) ) ;
#26253 = CARTESIAN_POINT ( 'NONE',  ( 0.4210617728738614285, -0.2437762437824630424, 0.1075369453634683753 ) ) ;
#26254 = EDGE_LOOP ( 'NONE', ( #18369, #15448, #14341, #534 ) ) ;
#26255 = DIRECTION ( 'NONE',  ( 1.000000000000000000, 0.000000000000000000, 0.000000000000000000 ) ) ;
#26256 = SHAPE_REPRESENTATION_RELATIONSHIP ( 'NONE' , 'NONE' ,  #26684, #10670 ) ;
#26257 = EDGE_LOOP ( 'NONE', ( #21354, #25380, #11846, #8139 ) ) ;
#26258 = CYLINDRICAL_SURFACE ( 'NONE', #4929, 0.6299212598425196763 ) ;
#26259 = B_SPLINE_CURVE_WITH_KNOTS ( 'NONE', 3,
 ( #27667, #22122, #24376, #5018 ),
 .UNSPECIFIED., .F., .F.,
 ( 4, 4 ),
 ( 0.3108507187342950395, 0.3125269569790670721 ),
 .UNSPECIFIED. ) ;
#26260 = FACE_OUTER_BOUND ( 'NONE', #19186, .T. ) ;
#26261 = LINE ( 'NONE', #17774, #27807 ) ;
#26262 = ORIENTED_EDGE ( 'NONE', *, *, #26620, .T. ) ;
#26263 = CARTESIAN_POINT ( 'NONE',  ( 0.3362148458988418187, -0.4382482975805321312, 0.9202755905511811330 ) ) ;
#26264 = FACE_BOUND ( 'NONE', #9430, .T. ) ;
#26265 = VERTEX_POINT ( 'NONE', #18331 ) ;
#26266 = CIRCLE ( 'NONE', #24911, 0.8163976377952752994 ) ;
#26267 = DIRECTION ( 'NONE',  ( 1.000000000000000000, 0.000000000000000000, 0.000000000000000000 ) ) ;
#26268 = VECTOR ( 'NONE', #18901, 39.37007874015748143 ) ;
#26269 = CARTESIAN_POINT ( 'NONE',  ( 0.6212598425196850238, 0.000000000000000000, 0.2574803149606298969 ) ) ;
#26270 = CYLINDRICAL_SURFACE ( 'NONE', #6683, 0.3771653543307086909 ) ;
#26271 = CYLINDRICAL_SURFACE ( 'NONE', #15169, 0.3722026523000413478 ) ;
#26272 = VECTOR ( 'NONE', #17720, 39.37007874015748143 ) ;
#26273 = CARTESIAN_POINT ( 'NONE',  ( -0.3751294191746890050, 0.2999672986753446069, 0.2529987172464028267 ) ) ;
#26274 = CARTESIAN_POINT ( 'NONE',  ( 0.4716107359500099072, 0.08256389912644751528, 0.08349695147423491504 ) ) ;
#26275 = CARTESIAN_POINT ( 'NONE',  ( -0.2421724791772047192, 0.2891474103999575052, 0.07637630750536809898 ) ) ;
#26276 = EDGE_CURVE ( 'NONE', #23913, #19458, #2514, .T. ) ;
#26277 = ORIENTED_EDGE ( 'NONE', *, *, #27539, .T. ) ;
#26278 = CARTESIAN_POINT ( 'NONE',  ( -0.09139240964747710749, -0.07874015748031500117, -1.188614124534770567E-17 ) ) ;
#26279 = CARTESIAN_POINT ( 'NONE',  ( -0.07472527936312729768, -0.5671862884094908130, 0.9399606299212598381 ) ) ;
#26280 = CARTESIAN_POINT ( 'NONE',  ( -0.4092783051644229841, -0.3145317858139328182, 1.766732283464566899 ) ) ;
#26281 = ORIENTED_EDGE ( 'NONE', *, *, #22714, .T. ) ;
#26282 = FACE_OUTER_BOUND ( 'NONE', #15411, .T. ) ;
#26283 = PRODUCT_DEFINITION_SHAPE ( 'NONE', 'NONE',  #27914 ) ;
#26284 = LINE ( 'NONE', #15571, #5636 ) ;
#26285 = B_SPLINE_CURVE_WITH_KNOTS ( 'NONE', 3,
 ( #6188, #4194, #14948, #1928, #23562, #12803, #21428, #14475, #3711, #12723 ),
 .UNSPECIFIED., .F., .F.,
 ( 4, 2, 2, 2, 4 ),
 ( 0.000000000000000000, 0.2500000000000000000, 0.5000000000000000000, 0.7500000000000000000, 1.000000000000000000 ),
 .UNSPECIFIED. ) ;
#26286 = DIRECTION ( 'NONE',  ( 1.000000000000000000, 0.000000000000000000, 0.000000000000000000 ) ) ;
#26287 = CONICAL_SURFACE ( 'NONE', #25837, 0.2362204724225640262, 0.2617993875000002579 ) ;
#26288 = CIRCLE ( 'NONE', #9134, 0.4226968503937005295 ) ;
#26289 = VERTEX_POINT ( 'NONE', #1131 ) ;
#26290 = VERTEX_POINT ( 'NONE', #26976 ) ;
#26291 = CARTESIAN_POINT ( 'NONE',  ( 0.000000000000000000, 0.1968503937007874127, 0.000000000000000000 ) ) ;
#26292 = CARTESIAN_POINT ( 'NONE',  ( -0.2230788859036007821, 0.2650812153444458419, 0.1377952755905510474 ) ) ;
#26293 = DIRECTION ( 'NONE',  ( -0.2225209339563147537, -0.9749279121818235083, 0.000000000000000000 ) ) ;
#26294 = ORIENTED_EDGE ( 'NONE', *, *, #9817, .T. ) ;
#26295 = FILL_AREA_STYLE ('',( #2289 ) ) ;
#26296 = DIRECTION ( 'NONE',  ( 1.000000000000000000, 0.000000000000000000, 0.000000000000000000 ) ) ;
#26297 = CARTESIAN_POINT ( 'NONE',  ( 0.7871730179869745880, 0.3051339520022200991, -0.1277767518403383762 ) ) ;
#26298 = CIRCLE ( 'NONE', #1956, 0.1110236220424516002 ) ;
#26299 = LINE ( 'NONE', #21662, #24292 ) ;
#26300 = ADVANCED_FACE ( 'NONE', ( #991 ), #2946, .F. ) ;
#26301 = VECTOR ( 'NONE', #15178, 39.37007874015748143 ) ;
#26302 = DIRECTION ( 'NONE',  ( 1.000000000000000000, 0.000000000000000000, 0.000000000000000000 ) ) ;
#26303 = EDGE_LOOP ( 'NONE', ( #9937, #22265, #6682, #14799, #25255 ) ) ;
#26304 = CARTESIAN_POINT ( 'NONE',  ( 0.07874015748031495954, -0.04546065111729338803, -0.3779527559055118058 ) ) ;
#26305 = CARTESIAN_POINT ( 'NONE',  ( 2.632951206231566310, 0.9448818897637796255, 0.1308464566929133654 ) ) ;
#26306 = CARTESIAN_POINT ( 'NONE',  ( 0.1327036767636011194, 0.4954415918535620689, -1.550196850393700920 ) ) ;
#26307 = ADVANCED_FACE ( 'NONE', ( #3079 ), #13346, .F. ) ;
#26308 = CARTESIAN_POINT ( 'NONE',  ( -0.1141732283464566844, 0.000000000000000000, 0.000000000000000000 ) ) ;
#26309 = ORIENTED_EDGE ( 'NONE', *, *, #27470, .F. ) ;
#26310 = CIRCLE ( 'NONE', #23169, 0.4786070381542913421 ) ;
#26311 = CARTESIAN_POINT ( 'NONE',  ( -0.2442565704126104242, 0.4954197419817720216, 0.9202755905511811330 ) ) ;
#26312 = AXIS2_PLACEMENT_3D ( 'NONE', #24257, #541, #26243 ) ;
#26313 = CARTESIAN_POINT ( 'NONE',  ( 0.3132247436407415431, 0.3723693495133243436, 0.09284957166292857889 ) ) ;
#26314 = AXIS2_PLACEMENT_3D ( 'NONE', #22267, #2899, #24802 ) ;
#26315 = CARTESIAN_POINT ( 'NONE',  ( -0.5781866216504639722, 0.4620966632784337391, 0.2562996995916987930 ) ) ;
#26316 = DIRECTION ( 'NONE',  ( 0.000000000000000000, 0.000000000000000000, 1.000000000000000000 ) ) ;
#26317 = FACE_OUTER_BOUND ( 'NONE', #1250, .T. ) ;
#26318 = LINE ( 'NONE', #8541, #511 ) ;
#26319 = CARTESIAN_POINT ( 'NONE',  ( 0.4256740239341992305, 0.5062356173701832995, 0.1926811207699622719 ) ) ;
#26320 = TOROIDAL_SURFACE ( 'NONE', #21814, 0.5610236220472440971, 0.1003937007874015908 ) ;
#26321 = EDGE_CURVE ( 'NONE', #13219, #4618, #5361, .T. ) ;
#26322 = CYLINDRICAL_SURFACE ( 'NONE', #9263, 0.4941010236220472751 ) ;
#26323 = LINE ( 'NONE', #11080, #18695 ) ;
#26324 = PLANE ( 'NONE',  #16501 ) ;
#26325 = EDGE_LOOP ( 'NONE', ( #18881, #14868 ) ) ;
#26326 = DIRECTION ( 'NONE',  ( 0.000000000000000000, 0.000000000000000000, 1.000000000000000000 ) ) ;
#26327 = ORIENTED_EDGE ( 'NONE', *, *, #11440, .T. ) ;
#26328 = CARTESIAN_POINT ( 'NONE',  ( -0.6912180915490531152, 0.1125275769341421150, 0.07327540503423307650 ) ) ;
#26329 = EDGE_LOOP ( 'NONE', ( #26873, #14835, #6765, #8082 ) ) ;
#26330 = AXIS2_PLACEMENT_3D ( 'NONE', #23030, #18768, #27686 ) ;
#26331 = CARTESIAN_POINT ( 'NONE',  ( -0.1574803149606299191, 0.5905511811023621549, 0.000000000000000000 ) ) ;
#26332 = CARTESIAN_POINT ( 'NONE',  ( 0.4061284506583976994, -0.2351468520617074898, 0.1992125984251968684 ) ) ;
#26333 = VECTOR ( 'NONE', #5219, 39.37007874015748143 ) ;
#26334 = FACE_OUTER_BOUND ( 'NONE', #24117, .T. ) ;
#26335 = CARTESIAN_POINT ( 'NONE',  ( 0.1970988029421506804, -0.3995913070740104711, -1.934055118110236560 ) ) ;
#26336 = CARTESIAN_POINT ( 'NONE',  ( -0.3726024258163779246, -0.02438677169354843896, -3.115157480314960647 ) ) ;
#26337 = LINE ( 'NONE', #15756, #25146 ) ;
#26338 = CARTESIAN_POINT ( 'NONE',  ( 0.000000000000000000, 0.000000000000000000, 0.09685039370078740717 ) ) ;
#26339 = CARTESIAN_POINT ( 'NONE',  ( 0.6239291699153675097, 0.1106940470467558946, 0.2481708550953252990 ) ) ;
#26340 = EDGE_CURVE ( 'NONE', #24033, #20796, #13789, .T. ) ;
#26341 = AXIS2_PLACEMENT_3D ( 'NONE', #26150, #15303, #16987 ) ;
#26342 = ORIENTED_EDGE ( 'NONE', *, *, #6294, .F. ) ;
#26343 = CARTESIAN_POINT ( 'NONE',  ( 0.000000000000000000, 0.000000000000000000, -0.1464516454673935042 ) ) ;
#26344 = VECTOR ( 'NONE', #3399, 39.37007874015748143 ) ;
#26345 = VERTEX_POINT ( 'NONE', #13760 ) ;
#26346 = AXIS2_PLACEMENT_3D ( 'NONE', #4759, #9000, #13654 ) ;
#26347 = CARTESIAN_POINT ( 'NONE',  ( 0.3916295560451238944, 0.3131429078216851902, 0.3080453759735494734 ) ) ;
#26348 = CARTESIAN_POINT ( 'NONE',  ( -0.4092783051644230397, 0.3145317858139328182, 1.766732283464566899 ) ) ;
#26349 = APPLICATION_PROTOCOL_DEFINITION ( 'draft international standard', 'automotive_design', 1998, #7843 ) ;
#26350 = CARTESIAN_POINT ( 'NONE',  ( -0.5118110236220472231, 0.03349795313264340019, 1.747047244094488194 ) ) ;
#26351 = VERTEX_POINT ( 'NONE', #7128 ) ;
#26352 = CARTESIAN_POINT ( 'NONE',  ( -0.1200583359873055728, 0.3535721684717720859, -3.115157480314960647 ) ) ;
#26353 = EDGE_LOOP ( 'NONE', ( #12994, #13183, #3367, #10828 ) ) ;
#26354 = DIRECTION ( 'NONE',  ( 0.000000000000000000, 1.000000000000000000, 0.000000000000000000 ) ) ;
#26355 = CARTESIAN_POINT ( 'NONE',  ( 0.4890020181331002358, -0.1109469068266557973, 0.1643955689295005795 ) ) ;
#26356 = AXIS2_PLACEMENT_3D ( 'NONE', #16675, #24856, #14579 ) ;
#26357 = CARTESIAN_POINT ( 'NONE',  ( 0.3239425792934479409, 0.08676778863010962961, 1.953740157480315043 ) ) ;
#26358 = ORIENTED_EDGE ( 'NONE', *, *, #21922, .F. ) ;
#26360 = EDGE_CURVE ( 'NONE', #1454, #24154, #3381, .T. ) ;
#26359 = EDGE_LOOP ( 'NONE', ( #7462, #5975, #3023, #10707, #24139, #19349 ) ) ;
#26361 = ORIENTED_EDGE ( 'NONE', *, *, #12383, .T. ) ;
#26362 = CARTESIAN_POINT ( 'NONE',  ( -0.4783464566929133688, 0.9448818897637796255, 0.1771653543307086520 ) ) ;
#26363 = VERTEX_POINT ( 'NONE', #11926 ) ;
#26364 = CARTESIAN_POINT ( 'NONE',  ( -0.06690352886863247528, -0.5085315017396038195, -1.550196850393700476 ) ) ;
#26365 = ORIENTED_EDGE ( 'NONE', *, *, #11726, .T. ) ;
#26366 = DIRECTION ( 'NONE',  ( 1.000000000000000000, 0.000000000000000000, 0.000000000000000000 ) ) ;
#26367 = AXIS2_PLACEMENT_3D ( 'NONE', #9745, #5226, #24857 ) ;
#26368 = EDGE_CURVE ( 'NONE', #19589, #25403, #13905, .T. ) ;
#26369 = CARTESIAN_POINT ( 'NONE',  ( -0.1786951194748074845, 1.015337136915029692, -0.5366467491745039453 ) ) ;
#26370 = CIRCLE ( 'NONE', #23249, 0.5007874015748031704 ) ;
#26371 = DIRECTION ( 'NONE',  ( 1.000000000000000000, 0.000000000000000000, 0.000000000000000000 ) ) ;
#26372 = DIRECTION ( 'NONE',  ( -1.000000000000000000, 0.000000000000000000, 0.000000000000000000 ) ) ;
#26373 = VERTEX_POINT ( 'NONE', #16311 ) ;
#26374 = DIRECTION ( 'NONE',  ( 0.000000000000000000, 0.000000000000000000, -1.000000000000000000 ) ) ;
#26375 = CARTESIAN_POINT ( 'NONE',  ( 0.1775730735577439323, 0.3074993854542599769, 1.953740157480315043 ) ) ;
#26376 = AXIS2_PLACEMENT_3D ( 'NONE', #11104, #26478, #22249 ) ;
#26377 = CARTESIAN_POINT ( 'NONE',  ( 0.000000000000000000, 0.000000000000000000, -0.1725236688546921415 ) ) ;
#26378 = CARTESIAN_POINT ( 'NONE',  ( 0.1504778549385778763, 0.2093060460840753811, -0.4379983118630946248 ) ) ;
#26379 = LINE ( 'NONE', #15929, #20688 ) ;
#26380 = DIRECTION ( 'NONE',  ( 0.000000000000000000, 0.000000000000000000, 1.000000000000000000 ) ) ;
#26381 = PLANE ( 'NONE',  #11035 ) ;
#26382 = AXIS2_PLACEMENT_3D ( 'NONE', #12403, #3927, #5015 ) ;
#26383 = DIRECTION ( 'NONE',  ( 0.000000000000000000, 1.000000000000000000, 0.000000000000000000 ) ) ;
#26384 = ORIENTED_EDGE ( 'NONE', *, *, #11853, .T. ) ;
#26385 = TOROIDAL_SURFACE ( 'NONE', #7006, 0.7165354330708662012, 0.01181102362204724393 ) ;
#26386 = CARTESIAN_POINT ( 'NONE',  ( -0.1968503937007874127, 0.8267716535433071723, 0.000000000000000000 ) ) ;
#26387 = EDGE_LOOP ( 'NONE', ( #3361, #5053 ) ) ;
#26388 = DIRECTION ( 'NONE',  ( -0.5000000010362839475, 0.000000000000000000, -0.8660254031861397417 ) ) ;
#26389 = EDGE_CURVE ( 'NONE', #6801, #14102, #1614, .T. ) ;
#26390 = VERTEX_POINT ( 'NONE', #15880 ) ;
#26391 = CARTESIAN_POINT ( 'NONE',  ( 0.000000000000000000, 0.000000000000000000, -0.05856299212598425896 ) ) ;
#26392 = DIRECTION ( 'NONE',  ( 0.000000000000000000, 0.000000000000000000, -1.000000000000000000 ) ) ;
#26393 = VERTEX_POINT ( 'NONE', #21374 ) ;
#26394 = CARTESIAN_POINT ( 'NONE',  ( 3.387491338582676985E-16, -0.6299212598425196763, -0.5915354330708662012 ) ) ;
#26395 = CARTESIAN_POINT ( 'NONE',  ( -0.1429116519061075785, -0.5335524835332366989, 0.9202755905511811330 ) ) ;
#26396 = ADVANCED_FACE ( 'NONE', ( #19387 ), #9737, .T. ) ;
#26397 = CIRCLE ( 'NONE', #15594, 0.1299232283464567261 ) ;
#26398 = CARTESIAN_POINT ( 'NONE',  ( -8.427884271297532088E-17, -0.6881889763779527325, 0.4062992125984251635 ) ) ;
#26399 = CARTESIAN_POINT ( 'NONE',  ( 0.4537304931026562849, 0.07942646906837143306, 0.1771653543307087630 ) ) ;
#26400 = EDGE_CURVE ( 'NONE', #8161, #10058, #5215, .T. ) ;
#26401 = CARTESIAN_POINT ( 'NONE',  ( 0.5869493968219645641, -0.2133897621573074832, 0.3696019098714952711 ) ) ;
#26402 = DIRECTION ( 'NONE',  ( 0.000000000000000000, 0.000000000000000000, -1.000000000000000000 ) ) ;
#26403 = CARTESIAN_POINT ( 'NONE',  ( -0.3661417322834645272, -0.4724409448818898127, 0.7100240035758484947 ) ) ;
#26404 = LINE ( 'NONE', #17521, #23721 ) ;
#26405 = CIRCLE ( 'NONE', #13324, 0.6881889763779527325 ) ;
#26406 = CARTESIAN_POINT ( 'NONE',  ( 0.7874015748031151229, 0.2490421840548274757, -0.2751330019808225780 ) ) ;
#26407 = AXIS2_PLACEMENT_3D ( 'NONE', #7358, #15977, #13856 ) ;
#26408 = CARTESIAN_POINT ( 'NONE',  ( 0.2041304421298504035, -0.2660793235464293249, 1.953740157480315043 ) ) ;
#26409 = ORIENTED_EDGE ( 'NONE', *, *, #24362, .T. ) ;
#26410 = CARTESIAN_POINT ( 'NONE',  ( 0.0005789221761214173069, 0.4692909815006417462, 0.07637795275590551769 ) ) ;
#26411 = CARTESIAN_POINT ( 'NONE',  ( 0.5417097841048850171, 0.1839420097223152528, 0.9399606299212598381 ) ) ;
#26412 = FACE_BOUND ( 'NONE', #16316, .T. ) ;
#26413 = DIRECTION ( 'NONE',  ( 1.000000000000000000, 0.000000000000000000, -0.000000000000000000 ) ) ;
#26414 = CARTESIAN_POINT ( 'NONE',  ( 0.3552064049866301976, 0.04673614183173152581, -3.115157480314960647 ) ) ;
#26415 = AXIS2_PLACEMENT_3D ( 'NONE', #10938, #19561, #19698 ) ;
#26416 = CARTESIAN_POINT ( 'NONE',  ( -0.0005939837304750000086, 0.5007870493127504208, 0.2574803149606298969 ) ) ;
#26417 = FACE_OUTER_BOUND ( 'NONE', #19303, .T. ) ;
#26418 = B_SPLINE_CURVE_WITH_KNOTS ( 'NONE', 3,
 ( #15564, #959, #24162, #9546, #23902, #20302 ),
 .UNSPECIFIED., .F., .F.,
 ( 4, 2, 4 ),
 ( 0.7157687286427140139, 0.7172350147555670574, 0.7187013008684189908 ),
 .UNSPECIFIED. ) ;
#26419 = ORIENTED_EDGE ( 'NONE', *, *, #9101, .F. ) ;
#26420 = ADVANCED_FACE ( 'NONE', ( #6403 ), #1179, .F. ) ;
#26421 = CARTESIAN_POINT ( 'NONE',  ( -0.1968503937007874127, 0.000000000000000000, 0.000000000000000000 ) ) ;
#26422 = AXIS2_PLACEMENT_3D ( 'NONE', #23480, #4110, #12710 ) ;
#26423 = CYLINDRICAL_SURFACE ( 'NONE', #13014, 0.8267716535433071723 ) ;
#26424 = ORIENTED_EDGE ( 'NONE', *, *, #5259, .T. ) ;
#26425 = EDGE_CURVE ( 'NONE', #20609, #14583, #23734, .T. ) ;
#26426 = DIRECTION ( 'NONE',  ( -1.000000000000000000, 0.000000000000000000, 0.000000000000000000 ) ) ;
#26427 = ORIENTED_EDGE ( 'NONE', *, *, #15192, .F. ) ;
#26428 = CIRCLE ( 'NONE', #14765, 0.08582677165167480748 ) ;
#26429 = CARTESIAN_POINT ( 'NONE',  ( 0.07874015748031495954, -0.04546065111729338803, -0.3779527559055118058 ) ) ;
#26430 = CARTESIAN_POINT ( 'NONE',  ( 0.7845931698711713365, 0.3958995273828118111, -0.1577356437548364521 ) ) ;
#26431 = DIRECTION ( 'NONE',  ( 0.1736481776669299981, -0.9848077530122081313, 0.000000000000000000 ) ) ;
#26432 = CARTESIAN_POINT ( 'NONE',  ( 0.000000000000000000, 0.000000000000000000, 0.1771653543307086520 ) ) ;
#26433 = ORIENTED_EDGE ( 'NONE', *, *, #20354, .T. ) ;
#26434 = FACE_OUTER_BOUND ( 'NONE', #3271, .T. ) ;
#26435 = CARTESIAN_POINT ( 'NONE',  ( -0.06441834428466408635, -0.4889536969035170877, -1.550196850393700920 ) ) ;
#26436 = CARTESIAN_POINT ( 'NONE',  ( 0.2031943647053979507, -0.4121342552748326060, -1.928289503579156960 ) ) ;
#26437 = CARTESIAN_POINT ( 'NONE',  ( 0.000000000000000000, 0.000000000000000000, 0.1771653543307086520 ) ) ;
#26438 = CARTESIAN_POINT ( 'NONE',  ( -0.07214854559198219386, 0.5476281405333177643, 0.9202755905511811330 ) ) ;
#26439 = CARTESIAN_POINT ( 'NONE',  ( 0.000000000000000000, 0.000000000000000000, 0.9399606299212598381 ) ) ;
#26440 = CYLINDRICAL_SURFACE ( 'NONE', #15522, 0.8267716535433071723 ) ;
#26441 = CARTESIAN_POINT ( 'NONE',  ( -0.4535326485287287657, 0.08054850140359764987, 0.1771653543307088186 ) ) ;
#26442 = DIRECTION ( 'NONE',  ( 1.000000000000000000, 0.000000000000000000, 0.000000000000000000 ) ) ;
#26443 = AXIS2_PLACEMENT_3D ( 'NONE', #18581, #2609, #20041 ) ;
#26444 = ORIENTED_EDGE ( 'NONE', *, *, #5142, .T. ) ;
#26445 = CARTESIAN_POINT ( 'NONE',  ( -0.6262477747318130339, -0.1078524472662568956, 0.2317403423130409423 ) ) ;
#26446 = CARTESIAN_POINT ( 'NONE',  ( 0.1716509673353401599, -0.4704508543867079173, 0.2574819596263889787 ) ) ;
#26447 = FILL_AREA_STYLE_COLOUR ( '', #2333 ) ;
#26448 = CARTESIAN_POINT ( 'NONE',  ( 0.3215969074633125979, 0.3838795254899315390, 0.2574819596263889787 ) ) ;
#26449 = EDGE_CURVE ( 'NONE', #17480, #9309, #1161, .T. ) ;
#26450 = CARTESIAN_POINT ( 'NONE',  ( -0.0006615832606325197825, 0.6212594902576319411, 0.09685039370078740717 ) ) ;
#26451 = EDGE_CURVE ( 'NONE', #11735, #1869, #15155, .T. ) ;
#26452 = DIRECTION ( 'NONE',  ( 0.7818314824680300257, 0.6234898018587330393, -0.000000000000000000 ) ) ;
#26453 = FACE_OUTER_BOUND ( 'NONE', #5652, .T. ) ;
#26454 = EDGE_CURVE ( 'NONE', #19648, #5266, #13770, .T. ) ;
#26455 = ORIENTED_EDGE ( 'NONE', *, *, #9380, .F. ) ;
#26456 = CARTESIAN_POINT ( 'NONE',  ( 0.1141145734057279204, 0.3362554559025014989, 1.953740157480315487 ) ) ;
#26457 = ORIENTED_EDGE ( 'NONE', *, *, #18967, .F. ) ;
#26458 = CARTESIAN_POINT ( 'NONE',  ( 0.4296318976989615401, 0.1458850421962473720, -1.934055118110236338 ) ) ;
#26459 = CARTESIAN_POINT ( 'NONE',  ( -0.3722026523000413478, 0.000000000000000000, -0.1756889763779527769 ) ) ;
#26460 = DIRECTION ( 'NONE',  ( 0.000000000000000000, 0.000000000000000000, -1.000000000000000000 ) ) ;
#26461 = CIRCLE ( 'NONE', #26038, 0.3593781546537452298 ) ;
#26462 = DIRECTION ( 'NONE',  ( 0.000000000000000000, 0.000000000000000000, 1.000000000000000000 ) ) ;
#26463 = CARTESIAN_POINT ( 'NONE',  ( 0.0005696707463081693290, 0.4606295689977896735, 0.1639447408819529051 ) ) ;
#26464 = AXIS2_PLACEMENT_3D ( 'NONE', #20088, #16409, #12311 ) ;
#26465 = PLANE ( 'NONE',  #1933 ) ;
#26466 = EDGE_CURVE ( 'NONE', #830, #7191, #26806, .T. ) ;
#26467 = CARTESIAN_POINT ( 'NONE',  ( 0.2488091035916884242, -0.2836590635674675620, -3.100567304031759175 ) ) ;
#26468 = LINE ( 'NONE', #26898, #14330 ) ;
#26469 = B_SPLINE_CURVE_WITH_KNOTS ( 'NONE', 3,
 ( #15928, #11683, #679, #26378, #7038, #26506, #13810, #2773 ),
 .UNSPECIFIED., .F., .F.,
 ( 4, 2, 2, 4 ),
 ( 0.000000000000000000, 0.2500000000000009437, 0.5000000000000018874, 1.000000000000000000 ),
 .UNSPECIFIED. ) ;
#26470 = LINE ( 'NONE', #19583, #4061 ) ;
#26471 = ADVANCED_FACE ( 'NONE', ( #13157 ), #7213, .F. ) ;
#26472 = ORIENTED_EDGE ( 'NONE', *, *, #10864, .F. ) ;
#26473 = CARTESIAN_POINT ( 'NONE',  ( 0.2965233727166233790, 0.3524965443697388734, 0.1771653543307087630 ) ) ;
#26474 = SHAPE_DEFINITION_REPRESENTATION ( #12737, #22737 ) ;
#26475 = CARTESIAN_POINT ( 'NONE',  ( -0.6722178168900768691, 0.03697663028270673641, -0.2369544657523791342 ) ) ;
#26476 = ORIENTED_EDGE ( 'NONE', *, *, #13492, .T. ) ;
#26477 = AXIS2_PLACEMENT_3D ( 'NONE', #24222, #16028, #2600 ) ;
#26478 = DIRECTION ( 'NONE',  ( 0.000000000000000000, 0.000000000000000000, 1.000000000000000000 ) ) ;
#26479 = LINE ( 'NONE', #5148, #16766 ) ;
#26480 = CARTESIAN_POINT ( 'NONE',  ( 0.5118110236220472231, 0.000000000000000000, 1.747047244094488194 ) ) ;
#26481 = EDGE_CURVE ( 'NONE', #22551, #12001, #4751, .T. ) ;
#26482 = CARTESIAN_POINT ( 'NONE',  ( -0.04877294052295848975, -0.3702005978258383068, -3.115157480314960647 ) ) ;
#26483 = ORIENTED_EDGE ( 'NONE', *, *, #18470, .T. ) ;
#26484 = DIRECTION ( 'NONE',  ( 1.000000000000000000, 0.000000000000000000, 0.000000000000000000 ) ) ;
#26485 = DIRECTION ( 'NONE',  ( 0.000000000000000000, 0.000000000000000000, -1.000000000000000000 ) ) ;
#26486 = EDGE_CURVE ( 'NONE', #16511, #16609, #874, .T. ) ;
#26487 = CARTESIAN_POINT ( 'NONE',  ( 0.2904160862623688666, 0.1677079028045472542, 1.953740157480315043 ) ) ;
#26488 = VERTEX_POINT ( 'NONE', #460 ) ;
#26489 = ORIENTED_EDGE ( 'NONE', *, *, #21994, .T. ) ;
#26490 = EDGE_CURVE ( 'NONE', #7191, #18194, #9698, .T. ) ;
#26491 = CARTESIAN_POINT ( 'NONE',  ( -0.6102362204724409711, 0.000000000000000000, 0.000000000000000000 ) ) ;
#26492 = VERTEX_POINT ( 'NONE', #24307 ) ;
#26493 = EDGE_LOOP ( 'NONE', ( #16127, #24863, #25225, #17438 ) ) ;
#26494 = VERTEX_POINT ( 'NONE', #13708 ) ;
#26495 = CARTESIAN_POINT ( 'NONE',  ( 0.02063739440522441987, 0.1968503937007874127, -3.624910829905205745 ) ) ;
#26496 = PRODUCT_DEFINITION_FORMATION_WITH_SPECIFIED_SOURCE ( 'ANY', '', #25356, .NOT_KNOWN. ) ;
#26497 = CARTESIAN_POINT ( 'NONE',  ( -0.4921259842519685179, 0.000000000000000000, -1.550196850393700920 ) ) ;
#26498 = AXIS2_PLACEMENT_3D ( 'NONE', #21248, #1465, #12627 ) ;
#26499 = FACE_OUTER_BOUND ( 'NONE', #25813, .T. ) ;
#26500 = CARTESIAN_POINT ( 'NONE',  ( 0.1522836969735573143, 0.4909267390297480382, 0.05591742528025173131 ) ) ;
#26501 = PRODUCT_DEFINITION_SHAPE ( 'NONE', 'NONE',  #27888 ) ;
#26502 = VECTOR ( 'NONE', #8107, 39.37007874015748143 ) ;
#26503 = LINE ( 'NONE', #1103, #9603 ) ;
#26504 = CARTESIAN_POINT ( 'NONE',  ( 0.04638120790932896698, -0.3520466617656974884, 1.953740157480315043 ) ) ;
#26505 = FACE_OUTER_BOUND ( 'NONE', #24933, .T. ) ;
#26506 = CARTESIAN_POINT ( 'NONE',  ( 0.1493295869868995207, 0.2235199554877277395, -0.4247682029637843693 ) ) ;
#26507 = CARTESIAN_POINT ( 'NONE',  ( -0.4167985568850881561, 0.07349283109919310664, 0.1377952755905511861 ) ) ;
#26508 = DIRECTION ( 'NONE',  ( 1.000000000000000000, 0.000000000000000000, 0.000000000000000000 ) ) ;
#26509 = CARTESIAN_POINT ( 'NONE',  ( 0.000000000000000000, 0.000000000000000000, 0.1377952755905511861 ) ) ;
#26510 = ADVANCED_BREP_SHAPE_REPRESENTATION ( 'Shaft Seal 20x35x7', ( #3022, #11588 ), #9813 ) ;
#26511 = AXIS2_PLACEMENT_3D ( 'NONE', #195, #2261, #8763 ) ;
#26512 = TOROIDAL_SURFACE ( 'NONE', #4866, 0.6102362204724409711, 0.1299212598425196763 ) ;
#26513 = DIRECTION ( 'NONE',  ( -0.9009688679024190350, -0.4338837391175581204, 0.000000000000000000 ) ) ;
#26514 = ORIENTED_EDGE ( 'NONE', *, *, #27124, .F. ) ;
#26515 = AXIS2_PLACEMENT_3D ( 'NONE', #3720, #8251, #18975 ) ;
#26516 = CARTESIAN_POINT ( 'NONE',  ( -2.685748425196850164E-17, 0.000000000000000000, -1.934055118110236338 ) ) ;
#26517 = ORIENTED_EDGE ( 'NONE', *, *, #10870, .T. ) ;
#26518 = CARTESIAN_POINT ( 'NONE',  ( -0.4066108233583291542, -0.2343118354750748089, 0.07637630773773071424 ) ) ;
#26519 = VERTEX_POINT ( 'NONE', #11590 ) ;
#26520 = FACE_OUTER_BOUND ( 'NONE', #12436, .T. ) ;
#26521 = CARTESIAN_POINT ( 'NONE',  ( -0.3346456692913385988, 4.268512490100411279E-17, 1.953740157480315043 ) ) ;
#26522 = CIRCLE ( 'NONE', #2639, 0.07874015748031489015 ) ;
#26523 = ORIENTED_EDGE ( 'NONE', *, *, #15727, .F. ) ;
#26524 = B_SPLINE_CURVE_WITH_KNOTS ( 'NONE', 3,
 ( #13961, #3481, #12109, #14540, #20868, #1111 ),
 .UNSPECIFIED., .F., .F.,
 ( 4, 2, 4 ),
 ( 0.000000000000000000, 0.5000000000000000000, 1.000000000000000000 ),
 .UNSPECIFIED. ) ;
#26525 = CARTESIAN_POINT ( 'NONE',  ( 0.4300830224589218820, 0.3772436174784425389, 0.9399606299212598381 ) ) ;
#26526 = ORIENTED_EDGE ( 'NONE', *, *, #20377, .T. ) ;
#26527 = CARTESIAN_POINT ( 'NONE',  ( -0.5393700787401575214, 6.677700066216866815E-17, 0.2755905511811023723 ) ) ;
#26528 = DIRECTION ( 'NONE',  ( 0.000000000000000000, -1.000000000000000000, 0.000000000000000000 ) ) ;
#26529 = CARTESIAN_POINT ( 'NONE',  ( 0.5610236220472440971, 0.000000000000000000, 0.1771653543307086520 ) ) ;
#26530 = CARTESIAN_POINT ( 'NONE',  ( -0.0002199787722797783896, 0.6212598425196852459, 0.09684793308443542803 ) ) ;
#26531 = CARTESIAN_POINT ( 'NONE',  ( 0.000000000000000000, 0.000000000000000000, 0.03818897637795275884 ) ) ;
#26532 = CARTESIAN_POINT ( 'NONE',  ( 0.5187889641967551313, -0.1190953285357214675, 0.1322834645669291320 ) ) ;
#26533 = AXIS2_PLACEMENT_3D ( 'NONE', #4499, #4227, #21463 ) ;
#26534 = AXIS2_PLACEMENT_3D ( 'NONE', #13560, #9307, #17911 ) ;
#26535 = CARTESIAN_POINT ( 'NONE',  ( 0.000000000000000000, 4.370956692913385731E-17, -8.195543307086614694E-17 ) ) ;
#26536 = CARTESIAN_POINT ( 'NONE',  ( -0.1220886091251831423, -0.3369140789106654932, 0.09506557084502520460 ) ) ;
#26537 = AXIS2_PLACEMENT_3D ( 'NONE', #3193, #9707, #16075 ) ;
#26538 = CARTESIAN_POINT ( 'NONE',  ( -0.3239425792934414461, 0.08676778863010937981, 1.953740157480315043 ) ) ;
#26539 = EDGE_CURVE ( 'NONE', #10634, #24154, #7089, .T. ) ;
#26540 = CARTESIAN_POINT ( 'NONE',  ( -0.5379714048901780288, 0.000000000000000000, -0.2342519685039370358 ) ) ;
#26541 = EDGE_CURVE ( 'NONE', #527, #7632, #17800, .T. ) ;
#26542 = CARTESIAN_POINT ( 'NONE',  ( 0.4066108233583291542, -0.2343118354750751975, 0.07637630773773071424 ) ) ;
#26543 = CARTESIAN_POINT ( 'NONE',  ( -2.685748425196850164E-17, 0.000000000000000000, -3.036417322828325105 ) ) ;
#26544 = PRODUCT_DEFINITION ( 'UNKNOWN', '', #20589, #4297 ) ;
#26545 = AXIS2_PLACEMENT_3D ( 'NONE', #3455, #22976, #24935 ) ;
#26546 = CARTESIAN_POINT ( 'NONE',  ( 0.000000000000000000, 0.000000000000000000, 0.2362204724409449064 ) ) ;
#26547 = DIRECTION ( 'NONE',  ( -1.000000000000000000, 0.000000000000000000, 0.000000000000000000 ) ) ;
#26548 = EDGE_CURVE ( 'NONE', #16795, #26747, #9251, .T. ) ;
#26549 = VERTEX_POINT ( 'NONE', #20070 ) ;
#26550 = ADVANCED_FACE ( 'NONE', ( #5232 ), #22330, .T. ) ;
#26551 = EDGE_CURVE ( 'NONE', #23339, #19765, #9316, .T. ) ;
#26552 = AXIS2_PLACEMENT_3D ( 'NONE', #12798, #19150, #21285 ) ;
#26553 = VERTEX_POINT ( 'NONE', #9461 ) ;
#26554 = AXIS2_PLACEMENT_3D ( 'NONE', #17816, #4971, #359 ) ;
#26555 = DIRECTION ( 'NONE',  ( 0.000000000000000000, 0.000000000000000000, -1.000000000000000000 ) ) ;
#26556 = CARTESIAN_POINT ( 'NONE',  ( -0.3062557396312245994, -0.6341756901071494701, 0.3281099440170536230 ) ) ;
#26557 = CIRCLE ( 'NONE', #877, 0.3937007874015748254 ) ;
#26558 = ORIENTED_EDGE ( 'NONE', *, *, #9918, .T. ) ;
#26559 = CARTESIAN_POINT ( 'NONE',  ( -0.5085329218535696860, 0.06689639104893733978, -1.550196850393700920 ) ) ;
#26560 = DIRECTION ( 'NONE',  ( -0.000000000000000000, 1.000000000000000000, -0.000000000000000000 ) ) ;
#26561 = VERTEX_POINT ( 'NONE', #9053 ) ;
#26562 = CARTESIAN_POINT ( 'NONE',  ( 0.4335958738490826581, -0.2505647196907697105, 0.2574827755769819038 ) ) ;
#26563 = VECTOR ( 'NONE', #26166, 39.37007874015748143 ) ;
#26564 = CARTESIAN_POINT ( 'NONE',  ( -0.1968503937007874127, -0.4724409448818898127, -0.8182917201112815953 ) ) ;
#26565 = CARTESIAN_POINT ( 'NONE',  ( 0.6175000359513720394, 0.5735261876549937465, -0.4659829881745126134 ) ) ;
#26566 = ORIENTED_EDGE ( 'NONE', *, *, #16824, .T. ) ;
#26567 = ORIENTED_EDGE ( 'NONE', *, *, #8524, .T. ) ;
#26568 = CARTESIAN_POINT ( 'NONE',  ( 0.3175540113612325133, 0.1078280746903942239, 1.973425196850393970 ) ) ;
#26569 = CARTESIAN_POINT ( 'NONE',  ( -0.1649135259639237794, 0.4856708409191340947, -1.550196850393700920 ) ) ;
#26570 = AXIS2_PLACEMENT_3D ( 'NONE', #11697, #16230, #13824 ) ;
#26571 = CARTESIAN_POINT ( 'NONE',  ( 0.2796934465393868807, 0.3645739570812638330, -1.928289503579156072 ) ) ;
#26572 = DIRECTION ( 'NONE',  ( 0.000000000000000000, 0.000000000000000000, 1.000000000000000000 ) ) ;
#26573 = AXIS2_PLACEMENT_3D ( 'NONE', #3759, #25661, #14945 ) ;
#26574 = CARTESIAN_POINT ( 'NONE',  ( 0.4783323773986568606, 0.2762247810518930202, 0.9202755905511811330 ) ) ;
#26575 = CARTESIAN_POINT ( 'NONE',  ( 0.6118978891064095205, 0.1074467966294586629, 0.2574819594177531479 ) ) ;
#26576 = ADVANCED_FACE ( 'NONE', ( #18054 ), #3100, .T. ) ;
#26577 = B_SPLINE_CURVE_WITH_KNOTS ( 'NONE', 3,
 ( #27587, #1174, #10612, #8503, #14890, #19517 ),
 .UNSPECIFIED., .F., .F.,
 ( 4, 2, 4 ),
 ( 0.2376120521391529850, 0.2390783382518560096, 0.2405446243645580073 ),
 .UNSPECIFIED. ) ;
#26578 = CARTESIAN_POINT ( 'NONE',  ( -0.3606190329934327310, 0.4297690281277732338, 0.1771653543307086520 ) ) ;
#26579 = AXIS2_PLACEMENT_3D ( 'NONE', #7677, #14180, #12708 ) ;
#26580 = CARTESIAN_POINT ( 'NONE',  ( -0.5510854067052418648, 0.4384931681296231898, 0.3281099440171127424 ) ) ;
#26581 = EDGE_CURVE ( 'NONE', #16756, #22088, #14259, .T. ) ;
#26582 = SHAPE_DEFINITION_REPRESENTATION ( #1221, #27787 ) ;
#26583 = PLANE ( 'NONE',  #1374 ) ;
#26584 = EDGE_CURVE ( 'NONE', #16610, #21046, #20096, .T. ) ;
#26585 = CARTESIAN_POINT ( 'NONE',  ( 0.2435608866411535234, 0.5103801548612577621, 0.1380420446583983662 ) ) ;
#26586 = DIRECTION ( 'NONE',  ( 0.000000000000000000, 0.000000000000000000, -1.000000000000000000 ) ) ;
#26587 = CARTESIAN_POINT ( 'NONE',  ( -0.5177165354330708347, 0.9448818897637796255, -9.561468503937007847E-18 ) ) ;
#26588 = CARTESIAN_POINT ( 'NONE',  ( -0.5579526598176230978, -0.3213561723287879368, 0.1183902030406979167 ) ) ;
#26589 = ( NAMED_UNIT ( * ) SI_UNIT ( $, .STERADIAN. ) SOLID_ANGLE_UNIT ( ) ) ;
#26590 = SPHERICAL_SURFACE ( 'NONE', #7044, 0.1003956692913385851 ) ;
#26591 = ORIENTED_EDGE ( 'NONE', *, *, #15914, .F. ) ;
#26593 = ADVANCED_FACE ( 'NONE', ( #17924 ), #17668, .T. ) ;
#26592 = CYLINDRICAL_SURFACE ( 'NONE', #22207, 0.8267716535433071723 ) ;
#26594 = ORIENTED_EDGE ( 'NONE', *, *, #3626, .F. ) ;
#26595 = CIRCLE ( 'NONE', #10355, 0.01377952755905511792 ) ;
#26596 = CYLINDRICAL_SURFACE ( 'NONE', #10218, 0.2395669291338582696 ) ;
#26597 = ADVANCED_FACE ( 'NONE', ( #24178 ), #4813, .F. ) ;
#26598 = ORIENTED_EDGE ( 'NONE', *, *, #23037, .F. ) ;
#26599 = CARTESIAN_POINT ( 'NONE',  ( 0.02963280468032034737, -0.4527559054764770385, -1.934055118110236338 ) ) ;
#26600 = CARTESIAN_POINT ( 'NONE',  ( -0.4333114377122877503, -0.2494818589555614918, 0.1259302777237963078 ) ) ;
#26601 = TOROIDAL_SURFACE ( 'NONE', #18950, 0.6102362204724409711, 0.1299212598425196763 ) ;
#26602 = CARTESIAN_POINT ( 'NONE',  ( -0.1606879121749082706, -0.4409237942971039881, 0.1992150590373740204 ) ) ;
#26603 = DIRECTION ( 'NONE',  ( 0.000000000000000000, 0.000000000000000000, 1.000000000000000000 ) ) ;
#26604 = CARTESIAN_POINT ( 'NONE',  ( -0.2362204724409449064, 0.000000000000000000, 0.000000000000000000 ) ) ;
#26605 = CARTESIAN_POINT ( 'NONE',  ( -0.5112608635011182123, 0.4674461882104614108, 0.01743336272964224679 ) ) ;
#26606 = AXIS2_PLACEMENT_3D ( 'NONE', #20076, #24311, #11320 ) ;
#26607 = DIRECTION ( 'NONE',  ( 0.000000000000000000, -1.000000000000000000, 0.000000000000000000 ) ) ;
#26608 = CARTESIAN_POINT ( 'NONE',  ( -0.3726024258163779246, 0.000000000000000000, -3.115157480314960647 ) ) ;
#26609 = CARTESIAN_POINT ( 'NONE',  ( 0.0001974756197917672956, 0.5007874015748032814, 0.09684793308443545579 ) ) ;
#26610 = CARTESIAN_POINT ( 'NONE',  ( 0.1490609433576163545, 0.2393035190829114200, 0.4144858534816307505 ) ) ;
#26611 = ORIENTED_EDGE ( 'NONE', *, *, #23370, .T. ) ;
#26612 = CARTESIAN_POINT ( 'NONE',  ( -0.2938049579018706114, 0.3349573549949406148, -1.934055118110236338 ) ) ;
#26613 = EDGE_CURVE ( 'NONE', #25691, #20032, #26874, .T. ) ;
#26614 = ADVANCED_FACE ( 'NONE', ( #9182 ), #23323, .F. ) ;
#26615 = APPLICATION_PROTOCOL_DEFINITION ( 'draft international standard', 'automotive_design', 1998, #12151 ) ;
#26616 = AXIS2_PLACEMENT_3D ( 'NONE', #14975, #19616, #27818 ) ;
#26617 = ORIENTED_EDGE ( 'NONE', *, *, #2902, .F. ) ;
#26618 = DIRECTION ( 'NONE',  ( 0.8660254037844382635, 0.5000000000000005551, 0.000000000000000000 ) ) ;
#26619 = CARTESIAN_POINT ( 'NONE',  ( -0.06699507805368211388, 0.5085118447801414421, 1.747047244094488194 ) ) ;
#26620 = EDGE_CURVE ( 'NONE', #18194, #12986, #15290, .T. ) ;
#26621 = ORIENTED_EDGE ( 'NONE', *, *, #23784, .F. ) ;
#26622 = FACE_BOUND ( 'NONE', #17500, .T. ) ;
#26623 = VERTEX_POINT ( 'NONE', #1561 ) ;
#26624 = AXIS2_PLACEMENT_3D ( 'NONE', #5311, #944, #13933 ) ;
#26625 = CARTESIAN_POINT ( 'NONE',  ( -0.3765118517642104257, 0.02464264302297881210, -3.100567304031763172 ) ) ;
#26626 = EDGE_LOOP ( 'NONE', ( #11122, #3208, #21739, #21016 ) ) ;
#26627 = CARTESIAN_POINT ( 'NONE',  ( 0.7874015748031496509, 0.3083957742196543061, -0.08983678263938775499 ) ) ;
#26628 = CARTESIAN_POINT ( 'NONE',  ( 0.1491281042588008532, 0.2475988972899728913, -0.4099885179503245936 ) ) ;
#26629 = CARTESIAN_POINT ( 'NONE',  ( 0.3346456692913385988, -0.02190250779246876237, 1.953740157480315043 ) ) ;
#26630 = ADVANCED_FACE ( 'NONE', ( #20493 ), #15184, .T. ) ;
#26631 = ORIENTED_EDGE ( 'NONE', *, *, #8001, .F. ) ;
#26632 = ORIENTED_EDGE ( 'NONE', *, *, #15206, .F. ) ;
#26633 = ORIENTED_EDGE ( 'NONE', *, *, #6112, .F. ) ;
#26634 = CARTESIAN_POINT ( 'NONE',  ( -0.3592839431930354710, -0.7102362189723434582, -0.6500175644856731605 ) ) ;
#26635 = CARTESIAN_POINT ( 'NONE',  ( -0.3986320731132244610, -0.2308081338369635804, 0.1771653543307087630 ) ) ;
#26636 = ORIENTED_EDGE ( 'NONE', *, *, #23876, .F. ) ;
#26637 = ORIENTED_EDGE ( 'NONE', *, *, #12567, .T. ) ;
#26638 = ORIENTED_EDGE ( 'NONE', *, *, #6004, .F. ) ;
#26639 = CARTESIAN_POINT ( 'NONE',  ( -0.6587140841000099778, 0.009105340598934882554, 0.2362204724409449064 ) ) ;
#26640 = AXIS2_PLACEMENT_3D ( 'NONE', #19147, #27780, #8693 ) ;
#26641 = CYLINDRICAL_SURFACE ( 'NONE', #4100, 0.1771653543307086798 ) ;
#26642 = CARTESIAN_POINT ( 'NONE',  ( -0.07667729696029146336, 0.1968503937007874405, -3.252002554478575558 ) ) ;
#26643 = CARTESIAN_POINT ( 'NONE',  ( -0.08530183727034107433, 0.03937007874015742426, -0.06819097667594002654 ) ) ;
#26644 = EDGE_CURVE ( 'NONE', #23447, #10256, #5954, .T. ) ;
#26645 = CIRCLE ( 'NONE', #11312, 0.1082677165354330728 ) ;
#26646 = CARTESIAN_POINT ( 'NONE',  ( 0.02576258704323619239, 0.2165354330708661734, -3.176774342847608068 ) ) ;
#26647 = DIRECTION ( 'NONE',  ( -3.508907999999997507E-18, 0.4999999999999998890, -0.8660254037844388186 ) ) ;
#26648 = CARTESIAN_POINT ( 'NONE',  ( 0.1570220809524471017, 0.3184841198566427112, 1.953740157480315043 ) ) ;
#26649 = EDGE_CURVE ( 'NONE', #10900, #17397, #25083, .T. ) ;
#26650 = LINE ( 'NONE', #1107, #24501 ) ;
#26651 = CARTESIAN_POINT ( 'NONE',  ( 0.1522836969735573143, -0.2938892803217901806, -0.3971963147566889840 ) ) ;
#26652 = DIRECTION ( 'NONE',  ( -1.000000000000000000, 0.000000000000000000, 0.000000000000000000 ) ) ;
#26653 = DIRECTION ( 'NONE',  ( -1.000000000000000000, 0.000000000000000000, 0.000000000000000000 ) ) ;
#26654 = CARTESIAN_POINT ( 'NONE',  ( 0.5043504886477625515, 0.1712563538832952981, 1.747047244094488194 ) ) ;
#26655 = CARTESIAN_POINT ( 'NONE',  ( 0.5085118447801419972, 0.06699507805369840641, 1.766732283464566899 ) ) ;
#26656 = VERTEX_POINT ( 'NONE', #7927 ) ;
#26657 = AXIS2_PLACEMENT_3D ( 'NONE', #7541, #1198, #26462 ) ;
#26658 = CARTESIAN_POINT ( 'NONE',  ( -0.03532354024591893848, -0.8267716535433071723, 0.000000000000000000 ) ) ;
#26659 = ORIENTED_EDGE ( 'NONE', *, *, #4744, .T. ) ;
#26660 = ADVANCED_FACE ( 'NONE', ( #25004 ), #5668, .T. ) ;
#26661 = DIRECTION ( 'NONE',  ( -1.000000000000000000, 0.000000000000000000, 0.000000000000000000 ) ) ;
#26662 = LENGTH_MEASURE_WITH_UNIT ( LENGTH_MEASURE( 0.02539999999999999897 ), #25115 ) ;
#26663 = CARTESIAN_POINT ( 'NONE',  ( -0.1141145734061086853, -0.3362554559022283285, 1.953740157480315043 ) ) ;
#26664 = ORIENTED_EDGE ( 'NONE', *, *, #27822, .T. ) ;
#26665 = CARTESIAN_POINT ( 'NONE',  ( -2.685748425196850164E-17, 0.000000000000000000, -1.934055118110236338 ) ) ;
#26666 = CONICAL_SURFACE ( 'NONE', #9065, 0.1106489370078740375, 0.08726646250000029414 ) ;
#26667 = B_SPLINE_CURVE_WITH_KNOTS ( 'NONE', 3,
 ( #18900, #12560, #3354, #16799, #27678, #20894 ),
 .UNSPECIFIED., .F., .F.,
 ( 4, 2, 4 ),
 ( 0.6902184472752670441, 0.6915327610580700446, 0.6928470748408730451 ),
 .UNSPECIFIED. ) ;
#26668 = CARTESIAN_POINT ( 'NONE',  ( 0.06441834428466665374, -0.4889536969035324088, -1.569881889763779625 ) ) ;
#26669 = CARTESIAN_POINT ( 'NONE',  ( 0.6993003464539847558, -0.1604063846364081614, 0.3122824329341128413 ) ) ;
#26670 = ORIENTED_EDGE ( 'NONE', *, *, #24202, .F. ) ;
#26671 = CARTESIAN_POINT ( 'NONE',  ( -0.1429116519060979196, -0.5335524835332288163, 0.9399606299212598381 ) ) ;
#26672 = ORIENTED_EDGE ( 'NONE', *, *, #19728, .T. ) ;
#26673 = VERTEX_POINT ( 'NONE', #16262 ) ;
#26674 = DIRECTION ( 'NONE',  ( -1.000000000000000000, 0.000000000000000000, 0.000000000000000000 ) ) ;
#26675 = CARTESIAN_POINT ( 'NONE',  ( 0.000000000000000000, 0.000000000000000000, -0.2755905511811023723 ) ) ;
#26676 = CARTESIAN_POINT ( 'NONE',  ( 0.1504778549386419362, 0.4839706879304455089, -0.03773480285758093467 ) ) ;
#26677 = CARTESIAN_POINT ( 'NONE',  ( -0.0004405150045870545247, 0.6212597256746517083, 0.09684874924366457249 ) ) ;
#26678 = DIRECTION ( 'NONE',  ( 0.000000000000000000, 1.000000000000000000, 0.000000000000000000 ) ) ;
#26679 = CIRCLE ( 'NONE', #6858, 0.3346456692913385988 ) ;
#26680 = VERTEX_POINT ( 'NONE', #25149 ) ;
#26681 = DIRECTION ( 'NONE',  ( 0.000000000000000000, 0.000000000000000000, 1.000000000000000000 ) ) ;
#26682 = EDGE_CURVE ( 'NONE', #24033, #12691, #10645, .T. ) ;
#26683 = EDGE_LOOP ( 'NONE', ( #22086, #27136, #9389, #18109 ) ) ;
#26684 = SHAPE_REPRESENTATION ( 'Deep Groove Ball Bearing 15x28x7', ( #11588 ), #2565 ) ;
#26685 = CARTESIAN_POINT ( 'NONE',  ( -0.05118110236220472370, 0.000000000000000000, 0.000000000000000000 ) ) ;
#26686 = CARTESIAN_POINT ( 'NONE',  ( 1.692913385826771533, 0.07874015748031491790, 3.109831496062992451E-16 ) ) ;
#26687 = CARTESIAN_POINT ( 'NONE',  ( -0.6259985246028595407, -0.1087303358534330439, 0.2316280589008344604 ) ) ;
#26688 = DIRECTION ( 'NONE',  ( -0.000000000000000000, -1.000000000000000000, -0.000000000000000000 ) ) ;
#26689 = DIRECTION ( 'NONE',  ( 0.000000000000000000, 0.000000000000000000, -1.000000000000000000 ) ) ;
#26690 = CARTESIAN_POINT ( 'NONE',  ( -4.821283464566928349E-18, 0.000000000000000000, -0.2834645669291338543 ) ) ;
#26691 = DIRECTION ( 'NONE',  ( -1.000000000000000000, 0.000000000000000000, 0.000000000000000000 ) ) ;
#26692 = ORIENTED_EDGE ( 'NONE', *, *, #3729, .F. ) ;
#26693 = DIRECTION ( 'NONE',  ( 0.000000000000000000, 0.000000000000000000, 1.000000000000000000 ) ) ;
#26694 = CONICAL_SURFACE ( 'NONE', #15523, 0.06200787401574806013, 0.5235987755983000369 ) ;
#26695 = ORIENTED_EDGE ( 'NONE', *, *, #10357, .T. ) ;
#26696 = AXIS2_PLACEMENT_3D ( 'NONE', #14566, #18617, #14272 ) ;
#26697 = DIRECTION ( 'NONE',  ( 0.000000000000000000, -1.000000000000000000, 0.000000000000000000 ) ) ;
#26698 = LINE ( 'NONE', #24437, #7590 ) ;
#26699 = CARTESIAN_POINT ( 'NONE',  ( 0.06048688226684505176, 0.1968503937008365401, -3.626935712454951943 ) ) ;
#26700 = VERTEX_POINT ( 'NONE', #27141 ) ;
#26701 = CARTESIAN_POINT ( 'NONE',  ( 0.000000000000000000, 0.000000000000000000, 0.2755905511811023723 ) ) ;
#26702 = ORIENTED_EDGE ( 'NONE', *, *, #5981, .F. ) ;
#26703 = EDGE_CURVE ( 'NONE', #6256, #23920, #6607, .T. ) ;
#26704 = AXIS2_PLACEMENT_3D ( 'NONE', #11433, #10250, #20190 ) ;
#26705 = ( NAMED_UNIT ( * ) SI_UNIT ( $, .STERADIAN. ) SOLID_ANGLE_UNIT ( ) ) ;
#26706 = CARTESIAN_POINT ( 'NONE',  ( 0.5309636003393858328, 0.6312391477623964242, -0.5378747345750526376 ) ) ;
#26707 = CARTESIAN_POINT ( 'NONE',  ( 0.2313841235333772006, 0.3010840436257775088, -3.100567304031763172 ) ) ;
#26708 = CARTESIAN_POINT ( 'NONE',  ( -0.3722026523000413478, 0.000000000000000000, -0.07578740157480315376 ) ) ;
#26709 = EDGE_CURVE ( 'NONE', #8922, #13827, #22382, .T. ) ;
#26710 = VERTEX_POINT ( 'NONE', #20916 ) ;
#26711 = ORIENTED_EDGE ( 'NONE', *, *, #20443, .T. ) ;
#26712 = CARTESIAN_POINT ( 'NONE',  ( -0.3239425792934402248, -0.08676778863011362641, 1.973425196850393970 ) ) ;
#26713 = B_SPLINE_CURVE_WITH_KNOTS ( 'NONE', 3,
 ( #3643, #1959, #12421, #5644, #1540, #14271 ),
 .UNSPECIFIED., .F., .F.,
 ( 4, 2, 4 ),
 ( 0.000000000000000000, 0.2500000000000000000, 0.5000000000000000000 ),
 .UNSPECIFIED. ) ;
#26714 = CARTESIAN_POINT ( 'NONE',  ( -0.1771653543307086520, -0.7539370078740157410, 9.233065434516462138E-17 ) ) ;
#26715 = CARTESIAN_POINT ( 'NONE',  ( -0.3707612262533164782, -0.3252100150720257377, -1.550196850393700920 ) ) ;
#26716 = TOROIDAL_SURFACE ( 'NONE', #15478, 0.1023622047244094474, 0.003937007874015747977 ) ;
#26717 = CARTESIAN_POINT ( 'NONE',  ( -0.5096726623837302128, -0.1170085733296502145, 0.3331434174568721485 ) ) ;
#26718 = CARTESIAN_POINT ( 'NONE',  ( 0.4954197419817712444, -0.2442565704126122561, 0.9202755905511811330 ) ) ;
#26719 = CYLINDRICAL_SURFACE ( 'NONE', #24267, 0.1771653543307086798 ) ;
#26720 = CARTESIAN_POINT ( 'NONE',  ( 0.1187185187227448868, -0.3276343780141734441, 0.1166443193830783709 ) ) ;
#26721 = CARTESIAN_POINT ( 'NONE',  ( -0.7874015748031496509, 0.000000000000000000, -1.052618110236220428 ) ) ;
#26722 = DIRECTION ( 'NONE',  ( 0.000000000000000000, 0.000000000000000000, 1.000000000000000000 ) ) ;
#26723 = LENGTH_MEASURE_WITH_UNIT ( LENGTH_MEASURE( 0.02539999999999999897 ), #18372 ) ;
#26724 = CARTESIAN_POINT ( 'NONE',  ( -0.1110236220424516002, 0.000000000000000000, 0.6299212598425196763 ) ) ;
#26725 = DIRECTION ( 'NONE',  ( 1.000000000000000000, 0.000000000000000000, 0.000000000000000000 ) ) ;
#26726 = DIRECTION ( 'NONE',  ( 0.000000000000000000, 1.000000000000000000, 0.000000000000000000 ) ) ;
#26727 = CARTESIAN_POINT ( 'NONE',  ( 0.1718374205099799101, -0.4703827404237102550, 0.2574803149606298969 ) ) ;
#26728 = VERTEX_POINT ( 'NONE', #5526 ) ;
#26729 = ORIENTED_EDGE ( 'NONE', *, *, #18002, .F. ) ;
#26730 = ADVANCED_FACE ( 'NONE', ( #1417 ), #24626, .F. ) ;
#26731 = DIRECTION ( 'NONE',  ( 0.000000000000000000, 0.000000000000000000, 1.000000000000000000 ) ) ;
#26732 = PRODUCT_DEFINITION_SHAPE ( 'NONE', 'NONE',  #6896 ) ;
#26733 = FACE_OUTER_BOUND ( 'NONE', #6466, .T. ) ;
#26734 = EDGE_LOOP ( 'NONE', ( #8839, #7748, #7355, #22786 ) ) ;
#26735 = VECTOR ( 'NONE', #24651, 39.37007874015748854 ) ;
#26736 = CARTESIAN_POINT ( 'NONE',  ( -8.919671568592927398E-17, -0.7283464566929134243, 0.3425196850393700809 ) ) ;
#26737 = ORIENTED_EDGE ( 'NONE', *, *, #26486, .F. ) ;
#26738 = CARTESIAN_POINT ( 'NONE',  ( -0.02963280468032184270, -0.4527559054764770385, -1.934055118110236338 ) ) ;
#26739 = CIRCLE ( 'NONE', #25878, 0.4986013261500205074 ) ;
#26740 = FACE_OUTER_BOUND ( 'NONE', #14750, .T. ) ;
#26741 = DIRECTION ( 'NONE',  ( 1.000000000000000000, 0.000000000000000000, 0.000000000000000000 ) ) ;
#26742 = CIRCLE ( 'NONE', #24052, 0.07677362204724411110 ) ;
#26743 = DIRECTION ( 'NONE',  ( -0.000000000000000000, -1.000000000000000000, -0.000000000000000000 ) ) ;
#26744 = PLANE ( 'NONE',  #909 ) ;
#26745 = CARTESIAN_POINT ( 'NONE',  ( 0.000000000000000000, 0.000000000000000000, 0.1377952755905511861 ) ) ;
#26746 = EDGE_CURVE ( 'NONE', #2008, #7423, #21536, .T. ) ;
#26747 = VERTEX_POINT ( 'NONE', #26844 ) ;
#26748 = DIRECTION ( 'NONE',  ( -0.000000000000000000, -1.000000000000000000, -0.000000000000000000 ) ) ;
#26749 = CIRCLE ( 'NONE', #14613, 0.01968503937007875723 ) ;
#26750 = CARTESIAN_POINT ( 'NONE',  ( -0.5949363243629232079, -0.1357903337134990229, 0.2362204724409449064 ) ) ;
#26751 = CARTESIAN_POINT ( 'NONE',  ( -0.04928467685643870416, 0.3740848232703742893, -3.100567304031763172 ) ) ;
#26753 = EDGE_CURVE ( 'NONE', #18631, #21933, #2086, .T. ) ;
#26752 = ( REPRESENTATION_RELATIONSHIP ('NONE','NONE', #12434, #6338 ) REPRESENTATION_RELATIONSHIP_WITH_TRANSFORMATION ( #9573 )SHAPE_REPRESENTATION_RELATIONSHIP( ) ) ;
#26754 = AXIS2_PLACEMENT_3D ( 'NONE', #15400, #5175, #24661 ) ;
#26755 = DIRECTION ( 'NONE',  ( 0.000000000000000000, 0.000000000000000000, 1.000000000000000000 ) ) ;
#26756 = CARTESIAN_POINT ( 'NONE',  ( 0.000000000000000000, 0.000000000000000000, 0.1322834645669291320 ) ) ;
#26757 = ORIENTED_EDGE ( 'NONE', *, *, #5617, .F. ) ;
#26758 = AXIS2_PLACEMENT_3D ( 'NONE', #7019, #15641, #24241 ) ;
#26759 = CARTESIAN_POINT ( 'NONE',  ( -0.4417361510194242613, -0.05819755867303597063, -1.934055118110236338 ) ) ;
#26760 = CLOSED_SHELL ( 'NONE', ( #3221, #733, #21156, #22615, #13773, #19466, #3028, #7111, #21118, #12933, #21402, #2078, #4902, #7314, #16743, #7304, #12907, #19477, #21861, #19712, #10723 ) ) ;
#26761 = DIRECTION ( 'NONE',  ( 0.000000000000000000, 0.000000000000000000, -1.000000000000000000 ) ) ;
#26762 = AXIS2_PLACEMENT_3D ( 'NONE', #19543, #19259, #24213 ) ;
#26763 = DIRECTION ( 'NONE',  ( 0.000000000000000000, 0.000000000000000000, 1.000000000000000000 ) ) ;
#26764 = DIRECTION ( 'NONE',  ( 0.000000000000000000, 0.000000000000000000, 1.000000000000000000 ) ) ;
#26765 = CARTESIAN_POINT ( 'NONE',  ( -0.2268096725222397969, 0.4600326175560398023, 1.747047244094488194 ) ) ;
#26766 = DIRECTION ( 'NONE',  ( 0.000000000000000000, 0.000000000000000000, -1.000000000000000000 ) ) ;
#26767 = ORIENTED_EDGE ( 'NONE', *, *, #17887, .F. ) ;
#26768 = TOROIDAL_SURFACE ( 'NONE', #18179, 0.5610236220472440971, 0.1003937007874015908 ) ;
#26769 = CARTESIAN_POINT ( 'NONE',  ( -0.02464264302293858039, -0.3765118517642103702, -3.100567304031763172 ) ) ;
#26770 = AXIS2_PLACEMENT_3D ( 'NONE', #12565, #25417, #25562 ) ;
#26771 = ORIENTED_EDGE ( 'NONE', *, *, #8518, .T. ) ;
#26772 = CARTESIAN_POINT ( 'NONE',  ( 0.7874015748031497619, 0.3568327973771865391, 0.06137828742325460857 ) ) ;
#26773 = CARTESIAN_POINT ( 'NONE',  ( 0.1120675189988346587, -0.7410715175625038897, 0.001857066358701141805 ) ) ;
#26774 = CARTESIAN_POINT ( 'NONE',  ( 0.3175540113612412840, -0.1078280746903980958, 1.953740157480315043 ) ) ;
#26775 = ORIENTED_EDGE ( 'NONE', *, *, #24362, .F. ) ;
#26776 = EDGE_LOOP ( 'NONE', ( #20834, #14060, #7572, #23408, #2072, #9926 ) ) ;
#26777 = EDGE_CURVE ( 'NONE', #16090, #11990, #10188, .T. ) ;
#26778 = CARTESIAN_POINT ( 'NONE',  ( -0.4055118110236220486, 0.9448818897637796255, -0.1308464566929134210 ) ) ;
#26779 = ORIENTED_EDGE ( 'NONE', *, *, #26551, .F. ) ;
#26780 = CARTESIAN_POINT ( 'NONE',  ( 0.5190862322091315262, -0.1177929122753177127, 0.1322834645669291320 ) ) ;
#26781 = VERTEX_POINT ( 'NONE', #7644 ) ;
#26782 = ORIENTED_EDGE ( 'NONE', *, *, #20571, .T. ) ;
#26783 = CARTESIAN_POINT ( 'NONE',  ( -0.7121770198535963825, 0.2056174084053519757, 0.2200249214779901596 ) ) ;
#26784 = CARTESIAN_POINT ( 'NONE',  ( -0.07668265949366928624, 0.1968503937007874127, -3.568865316179323788 ) ) ;
#26785 = EDGE_CURVE ( 'NONE', #21657, #10388, #4788, .T. ) ;
#26786 = CARTESIAN_POINT ( 'NONE',  ( 0.4898768902087983768, -3.235192913385827280E-16, -0.07874015748031495954 ) ) ;
#26787 = CARTESIAN_POINT ( 'NONE',  ( 0.07874015748031491790, 0.1968503937007874127, -3.262315100355583031 ) ) ;
#26788 = DIRECTION ( 'NONE',  ( -1.000000000000000000, 0.000000000000000000, 0.000000000000000000 ) ) ;
#26789 = CARTESIAN_POINT ( 'NONE',  ( -0.04380501567505456356, 0.3346456692913385988, 1.973425196850394192 ) ) ;
#26790 = CARTESIAN_POINT ( 'NONE',  ( -0.1771653543307086520, 0.000000000000000000, 0.000000000000000000 ) ) ;
#26791 = AXIS2_PLACEMENT_3D ( 'NONE', #335, #20068, #8912 ) ;
#26792 = FACE_OUTER_BOUND ( 'NONE', #2068, .T. ) ;
#26793 = CARTESIAN_POINT ( 'NONE',  ( -0.1968503937007874127, 0.07874015748031495954, -0.04546065111729338803 ) ) ;
#26794 = VECTOR ( 'NONE', #12568, 39.37007874015748143 ) ;
#26795 = CARTESIAN_POINT ( 'NONE',  ( -0.02319089060378155473, 0.3543307086614173596, 1.953740157480315043 ) ) ;
#26796 = EDGE_CURVE ( 'NONE', #13188, #24177, #5699, .T. ) ;
#26797 = VERTEX_POINT ( 'NONE', #10031 ) ;
#26798 = DIRECTION ( 'NONE',  ( -0.000000000000000000, -0.000000000000000000, -1.000000000000000000 ) ) ;
#26799 = DIRECTION ( 'NONE',  ( 0.000000000000000000, 1.000000000000000000, 0.000000000000000000 ) ) ;
#26800 = CARTESIAN_POINT ( 'NONE',  ( -0.3995066426835732765, 0.4757712504659606378, 0.09684793308443542803 ) ) ;
#26801 = DIRECTION ( 'NONE',  ( -0.9790454724845842893, 0.2036417511401760472, 0.000000000000000000 ) ) ;
#26802 = CARTESIAN_POINT ( 'NONE',  ( -0.3242071728275051634, -0.4225965726693019509, 1.747047244094488194 ) ) ;
#26803 = CARTESIAN_POINT ( 'NONE',  ( -0.2564944395515745823, 0.4441657790107744752, 1.766732283464566899 ) ) ;
#26804 = VECTOR ( 'NONE', #3657, 39.37007874015748143 ) ;
#26805 = ORIENTED_EDGE ( 'NONE', *, *, #4633, .F. ) ;
#26806 = ( BOUNDED_CURVE ( )  B_SPLINE_CURVE ( 2, ( #17131, #6677, #4550 ),
 .UNSPECIFIED., .F., .T. ) 
 B_SPLINE_CURVE_WITH_KNOTS ( ( 3, 3 ),
 ( 0.000000000000000000, 0.1168436138077914160 ),
 .UNSPECIFIED. ) 
 CURVE ( )  GEOMETRIC_REPRESENTATION_ITEM ( )  RATIONAL_B_SPLINE_CURVE ( ( 1.000000000000000000, 1.077350269189623067, 1.077350269189623067 ) ) 
 REPRESENTATION_ITEM ( '' )  ) ;
#26807 = DIRECTION ( 'NONE',  ( 0.000000000000000000, 0.000000000000000000, -1.000000000000000000 ) ) ;
#26808 = ORIENTED_EDGE ( 'NONE', *, *, #14701, .T. ) ;
#26809 = DIRECTION ( 'NONE',  ( 0.000000000000000000, 0.000000000000000000, 1.000000000000000000 ) ) ;
#26810 = CARTESIAN_POINT ( 'NONE',  ( 0.0005189969344232283309, 0.3771649972486724733, 0.1992125984251968684 ) ) ;
#26811 = LENGTH_MEASURE_WITH_UNIT ( LENGTH_MEASURE( 0.02539999999999999897 ), #17768 ) ;
#26812 = FACE_OUTER_BOUND ( 'NONE', #14716, .T. ) ;
#26813 = EDGE_LOOP ( 'NONE', ( #20006, #20781, #2497, #6162 ) ) ;
#26814 = EDGE_CURVE ( 'NONE', #21258, #13999, #2959, .T. ) ;
#26815 = CARTESIAN_POINT ( 'NONE',  ( -0.03220957031754079214, -0.4921259842519684624, -1.569881889763779625 ) ) ;
#26816 = CIRCLE ( 'NONE', #16437, 0.6614173228346456046 ) ;
#26817 = ORIENTED_EDGE ( 'NONE', *, *, #19240, .T. ) ;
#26818 = CARTESIAN_POINT ( 'NONE',  ( 0.4783323773986630778, -0.2762247810518744240, 0.9399606299212598381 ) ) ;
#26819 = ORIENTED_EDGE ( 'NONE', *, *, #5881, .F. ) ;
#26820 = EDGE_CURVE ( 'NONE', #14042, #23853, #27246, .T. ) ;
#26821 = DIRECTION ( 'NONE',  ( 0.000000000000000000, 0.000000000000000000, 1.000000000000000000 ) ) ;
#26822 = DIRECTION ( 'NONE',  ( 0.000000000000000000, 0.000000000000000000, -1.000000000000000000 ) ) ;
#26823 = CARTESIAN_POINT ( 'NONE',  ( -0.03532354024591893848, -0.8267716535433071723, 0.000000000000000000 ) ) ;
#26824 = DIRECTION ( 'NONE',  ( 0.000000000000000000, -1.000000000000000000, 0.000000000000000000 ) ) ;
#26825 = CARTESIAN_POINT ( 'NONE',  ( 0.2997912780622382090, -0.1736589463928937538, 0.1377952755905513249 ) ) ;
#26826 = CARTESIAN_POINT ( 'NONE',  ( -0.3041553300245938840, 0.09316743112151353035, 0.2362204724409449896 ) ) ;
#26827 = DIRECTION ( 'NONE',  ( -0.2036417511401758251, 0.4895227362422921447, -0.8478782506317885659 ) ) ;
#26828 = ADVANCED_FACE ( 'NONE', ( #6504 ), #12581, .T. ) ;
#26829 = AXIS2_PLACEMENT_3D ( 'NONE', #22860, #22710, #1517 ) ;
#26830 = CARTESIAN_POINT ( 'NONE',  ( -0.4133615125884808061, 0.4936731914940779564, 0.1183902030387112697 ) ) ;
#26831 = B_SPLINE_CURVE_WITH_KNOTS ( 'NONE', 3,
 ( #24021, #15012, #15150, #4534, #4398, #13004 ),
 .UNSPECIFIED., .F., .F.,
 ( 4, 2, 4 ),
 ( 0.000000000000000000, 0.2500000000000000000, 0.5000000000000000000 ),
 .UNSPECIFIED. ) ;
#26833 = ADVANCED_FACE ( 'NONE', ( #10588 ), #12906, .F. ) ;
#26832 = UNCERTAINTY_MEASURE_WITH_UNIT (LENGTH_MEASURE( 1.000000000000000082E-05 ), #24681, 'distance_accuracy_value', 'NONE') ;
#26834 = ORIENTED_EDGE ( 'NONE', *, *, #16048, .T. ) ;
#26835 = DIRECTION ( 'NONE',  ( -0.000000000000000000, -1.000000000000000000, -0.000000000000000000 ) ) ;
#26836 = CARTESIAN_POINT ( 'NONE',  ( -0.3012109481301850633, 0.3598698725862389813, 0.1992125984251968684 ) ) ;
#26837 = DIRECTION ( 'NONE',  ( -0.000000000000000000, -1.000000000000000000, -0.000000000000000000 ) ) ;
#26838 = AXIS2_PLACEMENT_3D ( 'NONE', #27084, #24658, #22697 ) ;
#26839 = DIRECTION ( 'NONE',  ( 1.000000000000000000, 0.000000000000000000, 0.000000000000000000 ) ) ;
#26840 = CYLINDRICAL_SURFACE ( 'NONE', #10580, 0.3937007874015748254 ) ;
#26841 = DIRECTION ( 'NONE',  ( 0.000000000000000000, -7.180547322999998243E-06, 0.9999999999742198442 ) ) ;
#26842 = AXIS2_PLACEMENT_3D ( 'NONE', #9559, #685, #7454 ) ;
#26843 = EDGE_LOOP ( 'NONE', ( #26670, #16655, #5496, #6407, #13038, #13637 ) ) ;
#26844 = CARTESIAN_POINT ( 'NONE',  ( -2.185478346456693112E-16, -0.8162224727389330026, 0.000000000000000000 ) ) ;
#26845 = DIRECTION ( 'NONE',  ( -1.000000000000000000, 0.000000000000000000, 0.000000000000000000 ) ) ;
#26846 = CARTESIAN_POINT ( 'NONE',  ( 0.09842519685039351207, 0.1968503937007873850, -3.548228346456693050 ) ) ;
#26847 = VERTEX_POINT ( 'NONE', #25579 ) ;
#26848 = ADVANCED_FACE ( 'NONE', ( #14998 ), #4524, .T. ) ;
#26849 = CARTESIAN_POINT ( 'NONE',  ( -0.8031496062992127261, 9.980389268641816488E-17, 0.4724409448818898127 ) ) ;
#26850 = VERTEX_POINT ( 'NONE', #27843 ) ;
#26851 = AXIS2_PLACEMENT_3D ( 'NONE', #25330, #12751, #14323 ) ;
#26852 = EDGE_CURVE ( 'NONE', #13490, #25509, #23885, .T. ) ;
#26853 = CARTESIAN_POINT ( 'NONE',  ( -0.1968503937007874127, 0.07874015748031495954, 0.04546065111729331171 ) ) ;
#26854 = CARTESIAN_POINT ( 'NONE',  ( 0.7873253891977465280, 0.2503290596427080739, -0.2788417078614053857 ) ) ;
#26855 = CARTESIAN_POINT ( 'NONE',  ( -0.04928528614549706338, 0.3765118517642103146, -3.100567304031762728 ) ) ;
#26856 = CARTESIAN_POINT ( 'NONE',  ( -1.692913385826771533, 0.4724409448818898127, -0.1181102362204721062 ) ) ;
#26857 = EDGE_LOOP ( 'NONE', ( #10486, #19534, #4738, #2887, #25574 ) ) ;
#26858 = CARTESIAN_POINT ( 'NONE',  ( -1.928513779527558736E-17, 0.000000000000000000, -0.02362204724409448786 ) ) ;
#26859 = EDGE_LOOP ( 'NONE', ( #25677, #3944 ) ) ;
#26860 = EDGE_LOOP ( 'NONE', ( #14742, #14836, #8624, #22226, #25130, #12551 ) ) ;
#26861 = CARTESIAN_POINT ( 'NONE',  ( 0.2211428102655756955, 0.2521176338356569957, 1.973425196850393970 ) ) ;
#26862 = CARTESIAN_POINT ( 'NONE',  ( -0.4889536969034878333, -0.06441834428466509943, -1.550196850393700920 ) ) ;
#26863 = CIRCLE ( 'NONE', #7470, 1.092519685039370136 ) ;
#26864 = CARTESIAN_POINT ( 'NONE',  ( -0.07214943758244271588, 0.5511811023622048555, 0.9202755905511812440 ) ) ;
#26865 = CARTESIAN_POINT ( 'NONE',  ( -0.2762247810519398716, 0.4783323773986303262, 0.9399606299212598381 ) ) ;
#26866 = LINE ( 'NONE', #23210, #8940 ) ;
#26867 = DIRECTION ( 'NONE',  ( 1.000000000000000000, 0.000000000000000000, 0.000000000000000000 ) ) ;
#26868 = VERTEX_POINT ( 'NONE', #21053 ) ;
#26869 = DIRECTION ( 'NONE',  ( 0.000000000000000000, 1.000000000000000000, 0.000000000000000000 ) ) ;
#26870 = EDGE_CURVE ( 'NONE', #27503, #12340, #26897, .T. ) ;
#26871 = CARTESIAN_POINT ( 'NONE',  ( 0.1275996891957681401, 0.4763861460130344172, -1.569881889763779625 ) ) ;
#26872 = CARTESIAN_POINT ( 'NONE',  ( 0.3010840436257777308, -0.2313841235333769231, -3.100567304031763616 ) ) ;
#26873 = ORIENTED_EDGE ( 'NONE', *, *, #17069, .F. ) ;
#26874 = CIRCLE ( 'NONE', #12466, 0.01181102362204730985 ) ;
#26875 = CARTESIAN_POINT ( 'NONE',  ( -0.3606190329934327310, 0.4297690281277732338, 0.1771653543307086520 ) ) ;
#26876 = FACE_OUTER_BOUND ( 'NONE', #20010, .T. ) ;
#26877 = DIRECTION ( 'NONE',  ( 0.000000000000000000, 1.000000000000000000, 0.000000000000000000 ) ) ;
#26878 = ORIENTED_EDGE ( 'NONE', *, *, #12083, .T. ) ;
#26879 = AXIS2_PLACEMENT_3D ( 'NONE', #23151, #1254, #18459 ) ;
#26880 = CARTESIAN_POINT ( 'NONE',  ( 0.0006679551606482677165, 0.5322830454629158270, 0.1322834645669291320 ) ) ;
#26881 = DIRECTION ( 'NONE',  ( 0.000000000000000000, 0.000000000000000000, 1.000000000000000000 ) ) ;
#26882 = B_SPLINE_CURVE_WITH_KNOTS ( 'NONE', 3,
 ( #23411, #8283, #6176, #12650, #10384, #19003 ),
 .UNSPECIFIED., .F., .F.,
 ( 4, 2, 4 ),
 ( 0.7157687286427130147, 0.7172350147555660582, 0.7187013008684189908 ),
 .UNSPECIFIED. ) ;
#26883 = VERTEX_POINT ( 'NONE', #23614 ) ;
#26884 = CARTESIAN_POINT ( 'NONE',  ( -0.03532354024591775193, -0.6299212598425196763, 0.5531496062992126150 ) ) ;
#26885 = EDGE_LOOP ( 'NONE', ( #23320, #16789, #25068, #25785 ) ) ;
#26886 = CARTESIAN_POINT ( 'NONE',  ( 0.3599896729929412120, -0.2761764805255614297, -1.934055118110236338 ) ) ;
#26887 = CARTESIAN_POINT ( 'NONE',  ( -0.4067073728345788064, -0.2341441294389334793, 0.1992125984251968684 ) ) ;
#26888 = FACE_OUTER_BOUND ( 'NONE', #22008, .T. ) ;
#26889 = CARTESIAN_POINT ( 'NONE',  ( 2.664928230027803213, -0.4724409448818898127, -0.7100240035758484947 ) ) ;
#26890 = CARTESIAN_POINT ( 'NONE',  ( 0.3714653163189441387, 0.06532421472592657430, 0.07637549214372835182 ) ) ;
#26891 = CARTESIAN_POINT ( 'NONE',  ( 0.5118110236220473341, 6.402768735150616610E-17, -1.550196850393700920 ) ) ;
#26892 = ORIENTED_EDGE ( 'NONE', *, *, #10571, .F. ) ;
#26893 = CARTESIAN_POINT ( 'NONE',  ( 0.4622619257814346572, 0.08092139668567618904, 0.07637795275590551769 ) ) ;
#26894 = CARTESIAN_POINT ( 'NONE',  ( 0.6791338582677166613, 0.6883602804966771904, 0.000000000000000000 ) ) ;
#26895 = ORIENTED_EDGE ( 'NONE', *, *, #3260, .F. ) ;
#26896 = CARTESIAN_POINT ( 'NONE',  ( -0.3572819248074403653, -0.1213180142433946673, -3.100567304031765392 ) ) ;
#26897 = CIRCLE ( 'NONE', #17420, 0.01377952755905511965 ) ;
#26898 = CARTESIAN_POINT ( 'NONE',  ( 0.4842519685039370358, 5.930376232091513698E-17, -0.1309055118110236116 ) ) ;
#26899 = DIRECTION ( 'NONE',  ( 0.000000000000000000, 0.000000000000000000, -1.000000000000000000 ) ) ;
#26900 = PRODUCT_DEFINITION_CONTEXT ( 'detailed design', #7843, 'design' ) ;
#26901 = ORIENTED_EDGE ( 'NONE', *, *, #4307, .F. ) ;
#26902 = CARTESIAN_POINT ( 'NONE',  ( -0.3349573549949665940, -0.2938049579018697788, -1.934055118110236338 ) ) ;
#26903 = AXIS2_PLACEMENT_3D ( 'NONE', #23222, #12472, #21086 ) ;
#26904 = ADVANCED_FACE ( 'NONE', ( #2252, #12851 ), #1978, .T. ) ;
#26905 = CARTESIAN_POINT ( 'NONE',  ( -0.4121342552748409327, 0.2031943647053852109, -1.928289503579154074 ) ) ;
#26906 = EDGE_CURVE ( 'NONE', #14713, #22576, #21193, .T. ) ;
#26907 = ADVANCED_FACE ( 'NONE', ( #17238 ), #14763, .F. ) ;
#26908 = B_SPLINE_CURVE_WITH_KNOTS ( 'NONE', 3,
 ( #27286, #25447, #10321, #12160, #16406, #14159 ),
 .UNSPECIFIED., .F., .F.,
 ( 4, 2, 4 ),
 ( 0.9031406754215579591, 0.9046454396443720514, 0.9061502038671850334 ),
 .UNSPECIFIED. ) ;
#26909 = VERTEX_POINT ( 'NONE', #25436 ) ;
#26910 = PRODUCT_RELATED_PRODUCT_CATEGORY ( 'part', '', ( #2147 ) ) ;
#26911 = CARTESIAN_POINT ( 'NONE',  ( 0.09842519685039370636, 0.2165354330708661457, -3.456364829396327387 ) ) ;
#26912 = CARTESIAN_POINT ( 'NONE',  ( 0.000000000000000000, 0.000000000000000000, -0.4724409448841456749 ) ) ;
#26913 = CARTESIAN_POINT ( 'NONE',  ( 0.3382184156732163660, 0.3855916753051394363, 1.747047244094488194 ) ) ;
#26914 = EDGE_CURVE ( 'NONE', #8934, #4649, #2534, .T. ) ;
#26915 = PRESENTATION_STYLE_ASSIGNMENT (( #22253 ) ) ;
#26916 = ORIENTED_EDGE ( 'NONE', *, *, #18282, .T. ) ;
#26917 = AXIS2_PLACEMENT_3D ( 'NONE', #24769, #5435, #16025 ) ;
#26918 = ORIENTED_EDGE ( 'NONE', *, *, #11834, .F. ) ;
#26919 = CARTESIAN_POINT ( 'NONE',  ( 0.09762295995069844579, 0.3644697409450269321, -3.100567304031763172 ) ) ;
#26920 = ADVANCED_FACE ( 'NONE', ( #16965 ), #25564, .T. ) ;
#26921 = CIRCLE ( 'NONE', #15207, 0.8267716535433071723 ) ;
#26922 = EDGE_CURVE ( 'NONE', #24718, #5673, #4781, .T. ) ;
#26923 = ORIENTED_EDGE ( 'NONE', *, *, #17561, .F. ) ;
#26924 = DIRECTION ( 'NONE',  ( 0.000000000000000000, 1.000000000000000000, 0.000000000000000000 ) ) ;
#26925 = DIRECTION ( 'NONE',  ( 1.000000000000000000, 0.000000000000000000, 0.000000000000000000 ) ) ;
#26926 = ORIENTED_EDGE ( 'NONE', *, *, #5794, .T. ) ;
#26927 = CARTESIAN_POINT ( 'NONE',  ( 0.1648275707509661014, 0.4857079805365772107, -1.550196850393701142 ) ) ;
#26928 = AXIS2_PLACEMENT_3D ( 'NONE', #21963, #495, #24212 ) ;
#26929 = PLANE ( 'NONE',  #6733 ) ;
#26930 = DIRECTION ( 'NONE',  ( 0.000000000000000000, 0.000000000000000000, 1.000000000000000000 ) ) ;
#26931 = VERTEX_POINT ( 'NONE', #559 ) ;
#26932 = CARTESIAN_POINT ( 'NONE',  ( -0.1152775731717075036, 0.4303822302054133853, -1.934055118110236338 ) ) ;
#26933 = ORIENTED_EDGE ( 'NONE', *, *, #3133, .F. ) ;
#26934 = ORIENTED_EDGE ( 'NONE', *, *, #26245, .F. ) ;
#26935 = CARTESIAN_POINT ( 'NONE',  ( -0.4446020952038907681, 0.000000000000000000, -1.934055118110236338 ) ) ;
#26936 = FACE_OUTER_BOUND ( 'NONE', #9566, .T. ) ;
#26937 = CARTESIAN_POINT ( 'NONE',  ( 0.000000000000000000, 0.000000000000000000, 0.1771653543307086520 ) ) ;
#26938 = DIRECTION ( 'NONE',  ( -0.9790454724845842893, -0.2036417511401760472, 2.493892000000000781E-17 ) ) ;
#26939 = CARTESIAN_POINT ( 'NONE',  ( -0.3722026523000413478, 0.000000000000000000, -0.2204724409448818867 ) ) ;
#26940 = CARTESIAN_POINT ( 'NONE',  ( -0.08759279594700326854, 0.3259357382551448246, 1.973425196850393526 ) ) ;
#26941 = CARTESIAN_POINT ( 'NONE',  ( 0.5925575908939920700, 0.4537419570391968415, 0.000000000000000000 ) ) ;
#26942 = CARTESIAN_POINT ( 'NONE',  ( 0.000000000000000000, 0.000000000000000000, 0.1377952755905511861 ) ) ;
#26943 = ( GEOMETRIC_REPRESENTATION_CONTEXT ( 3 ) GLOBAL_UNCERTAINTY_ASSIGNED_CONTEXT ( ( #11857 ) ) GLOBAL_UNIT_ASSIGNED_CONTEXT ( ( #3369, #18633, #5664 ) ) REPRESENTATION_CONTEXT ( 'NONE', 'WORKASPACE' ) ) ;
#26944 = CARTESIAN_POINT ( 'NONE',  ( 0.2056553984168021654, -0.2676050456844303316, 1.973425196850393970 ) ) ;
#26945 = CARTESIAN_POINT ( 'NONE',  ( 0.09187177619659094019, 0.3429980251342388264, 1.953740157480315043 ) ) ;
#26946 = ORIENTED_EDGE ( 'NONE', *, *, #2035, .T. ) ;
#26947 = CARTESIAN_POINT ( 'NONE',  ( -4.821283464566928349E-18, 0.000000000000000000, -0.02362204724409468909 ) ) ;
#26948 = EDGE_CURVE ( 'NONE', #12947, #4526, #22298, .T. ) ;
#26949 = CARTESIAN_POINT ( 'NONE',  ( 0.3992017438595159562, -0.2298214351608004746, 0.1771653543307084855 ) ) ;
#26950 = CARTESIAN_POINT ( 'NONE',  ( -0.2307489990847578776, -0.4796672131996535526, 0.1322810039474933141 ) ) ;
#26951 = ORIENTED_EDGE ( 'NONE', *, *, #16272, .T. ) ;
#26952 = CARTESIAN_POINT ( 'NONE',  ( -5.747161356628524594E-17, -0.4692913385826771866, 0.2755905511811023723 ) ) ;
#26953 = DIRECTION ( 'NONE',  ( 0.000000000000000000, -1.000000000000000000, 0.000000000000000000 ) ) ;
#26954 = CARTESIAN_POINT ( 'NONE',  ( -0.3512268162760395773, 0.4004221243553298115, 1.747047244094488194 ) ) ;
#26955 = ADVANCED_FACE ( 'NONE', ( #6923 ), #21036, .F. ) ;
#26956 = CARTESIAN_POINT ( 'NONE',  ( 0.5118110236220472231, 0.000000000000000000, 1.766732283464566899 ) ) ;
#26957 = VERTEX_POINT ( 'NONE', #24546 ) ;
#26958 = CARTESIAN_POINT ( 'NONE',  ( -0.09139240964747699647, 0.07874015748031500117, -0.02109836160874975844 ) ) ;
#26959 = ORIENTED_EDGE ( 'NONE', *, *, #6538, .T. ) ;
#26961 = EDGE_CURVE ( 'NONE', #19454, #27117, #6334, .T. ) ;
#26960 = DIRECTION ( 'NONE',  ( 0.000000000000000000, 1.000000000000000000, 0.000000000000000000 ) ) ;
#26962 = CARTESIAN_POINT ( 'NONE',  ( 0.6708219662590886312, -0.1536294932067318875, 0.3401591245381555551 ) ) ;
#26963 = LINE ( 'NONE', #14555, #24012 ) ;
#26964 = CIRCLE ( 'NONE', #14814, 0.1476377952755905387 ) ;
#26965 = DIRECTION ( 'NONE',  ( -1.000000000000000000, 0.000000000000000000, 0.000000000000000000 ) ) ;
#26966 = ORIENTED_EDGE ( 'NONE', *, *, #14413, .F. ) ;
#26967 = ORIENTED_EDGE ( 'NONE', *, *, #23544, .T. ) ;
#26968 = CARTESIAN_POINT ( 'NONE',  ( -0.3252100150720236282, -0.3707612262533184766, -1.569881889763779625 ) ) ;
#26969 = CIRCLE ( 'NONE', #10255, 0.7539370078740157410 ) ;
#26970 = EDGE_LOOP ( 'NONE', ( #25392, #23102, #14563, #8440 ) ) ;
#26971 = ORIENTED_EDGE ( 'NONE', *, *, #14413, .T. ) ;
#26972 = EDGE_CURVE ( 'NONE', #16738, #935, #27355, .T. ) ;
#26973 = DIRECTION ( 'NONE',  ( -1.000000000000000000, 0.000000000000000000, 0.000000000000000000 ) ) ;
#26974 = CARTESIAN_POINT ( 'NONE',  ( -0.1589886963208103077, -0.4351482077921629554, 0.2048502515415793201 ) ) ;
#26975 = CARTESIAN_POINT ( 'NONE',  ( 0.1518453843511950729, 0.4909359254672716610, 0.05583672882996252446 ) ) ;
#26976 = CARTESIAN_POINT ( 'NONE',  ( 0.000000000000000000, -1.707404996040164512E-16, -0.3937007874015748254 ) ) ;
#26977 = CARTESIAN_POINT ( 'NONE',  ( -0.4222761783096392052, 0.5043089796487417731, 0.1461456498289284978 ) ) ;
#26978 = CARTESIAN_POINT ( 'NONE',  ( -0.2041304421298407168, -0.2660793235464189999, 1.953740157480315043 ) ) ;
#26979 = CONICAL_SURFACE ( 'NONE', #13899, 0.1110236220424516002, 0.7853981642948906217 ) ;
#26980 = VERTEX_POINT ( 'NONE', #8889 ) ;
#26981 = LINE ( 'NONE', #26540, #1062 ) ;
#26982 = DIRECTION ( 'NONE',  ( 0.000000000000000000, 0.000000000000000000, -1.000000000000000000 ) ) ;
#26983 = AXIS2_PLACEMENT_3D ( 'NONE', #3256, #24598, #24742 ) ;
#26984 = VECTOR ( 'NONE', #16310, 39.37007874015748143 ) ;
#26985 = CARTESIAN_POINT ( 'NONE',  ( 0.2131049448084480213, -0.5835666837866708700, 0.2574803149606298969 ) ) ;
#26987 = LINE ( 'NONE', #16115, #27285 ) ;
#26988 = EDGE_CURVE ( 'NONE', #20147, #23745, #18028, .T. ) ;
#26989 = DIRECTION ( 'NONE',  ( 0.000000000000000000, 0.000000000000000000, -1.000000000000000000 ) ) ;
#26990 = CIRCLE ( 'NONE', #12561, 0.4807043897637795493 ) ;
#26991 = ORIENTED_EDGE ( 'NONE', *, *, #25712, .T. ) ;
#26992 = CARTESIAN_POINT ( 'NONE',  ( -0.5187889641967551313, -0.1190953285357212593, 0.3401574803149606252 ) ) ;
#26993 = ADVANCED_FACE ( 'NONE', ( #13128 ), #837, .F. ) ;
#26994 = B_SPLINE_CURVE_WITH_KNOTS ( 'NONE', 3,
 ( #14452, #18360, #20787, #23062, #27579, #9906, #12162, #18793, #25017, #5684 ),
 .UNSPECIFIED., .F., .F.,
 ( 4, 2, 2, 2, 4 ),
 ( 0.000000000000000000, 0.2500000000000000000, 0.5000000000000000000, 0.7500000000000000000, 1.000000000000000000 ),
 .UNSPECIFIED. ) ;
#26995 = ORIENTED_EDGE ( 'NONE', *, *, #26007, .F. ) ;
#26996 = CARTESIAN_POINT ( 'NONE',  ( 0.000000000000000000, 0.000000000000000000, 0.07637795275590551769 ) ) ;
#26997 = FACE_OUTER_BOUND ( 'NONE', #8990, .T. ) ;
#26998 = ORIENTED_EDGE ( 'NONE', *, *, #9420, .T. ) ;
#26999 = CARTESIAN_POINT ( 'NONE',  ( -0.09586345222255253373, 0.1968503937007873850, -3.573990933995847996 ) ) ;
#27000 = ORIENTED_EDGE ( 'NONE', *, *, #23302, .F. ) ;
#27001 = CARTESIAN_POINT ( 'NONE',  ( -0.3856588814717645808, 0.3381532161291478378, -1.550196850393700476 ) ) ;
#27002 = DIRECTION ( 'NONE',  ( 0.000000000000000000, 1.000000000000000000, 0.000000000000000000 ) ) ;
#27003 = EDGE_LOOP ( 'NONE', ( #14735, #18843 ) ) ;
#27004 = CONICAL_SURFACE ( 'NONE', #850, 0.4055307389460929279, 0.3230892413134540120 ) ;
#27005 = DIRECTION ( 'NONE',  ( 0.000000000000000000, 0.000000000000000000, 1.000000000000000000 ) ) ;
#27006 = AXIS2_PLACEMENT_3D ( 'NONE', #10755, #21499, #6522 ) ;
#27007 = CIRCLE ( 'NONE', #16181, 0.7283464566929134243 ) ;
#27008 = CARTESIAN_POINT ( 'NONE',  ( -1.197070535079588716, 0.07874015748031491790, 1.315180771300060503 ) ) ;
#27009 = DIRECTION ( 'NONE',  ( 1.000000000000000000, 0.000000000000000000, 0.000000000000000000 ) ) ;
#27010 = CARTESIAN_POINT ( 'NONE',  ( 0.000000000000000000, 0.4724409448818898127, -0.4921259842519685179 ) ) ;
#27011 = VERTEX_POINT ( 'NONE', #15547 ) ;
#27012 = AXIS2_PLACEMENT_3D ( 'NONE', #23681, #17442, #6853 ) ;
#27013 = VERTEX_POINT ( 'NONE', #21757 ) ;
#27014 = CARTESIAN_POINT ( 'NONE',  ( -0.3346456692913385988, 0.02190250779246044610, 1.973425196850393970 ) ) ;
#27015 = CARTESIAN_POINT ( 'NONE',  ( -0.3382184156749069581, -0.3855916753034488997, -1.550196850393700920 ) ) ;
#27016 = CARTESIAN_POINT ( 'NONE',  ( 0.4816145447621894560, 0.2775852647713619170, 0.9202755905511812440 ) ) ;
#27018 = EDGE_CURVE ( 'NONE', #26781, #20698, #26261, .T. ) ;
#27017 = CARTESIAN_POINT ( 'NONE',  ( 0.03001016326913514068, -0.4585215200179055817, -1.928289503579156516 ) ) ;
#27019 = CARTESIAN_POINT ( 'NONE',  ( 0.03607471876262385857, -0.5511811023622048555, 0.9202755905511811330 ) ) ;
#27020 = CARTESIAN_POINT ( 'NONE',  ( 0.0004974201395668471654, 0.3464563358313494934, 0.1377952755905513249 ) ) ;
#27021 = CARTESIAN_POINT ( 'NONE',  ( 0.000000000000000000, 0.000000000000000000, 0.2574803149606298969 ) ) ;
#27022 = VERTEX_POINT ( 'NONE', #15674 ) ;
#27023 = CARTESIAN_POINT ( 'NONE',  ( -0.2307489990847578776, -0.4796672131996535526, 0.3401599409343964431 ) ) ;
#27024 = ADVANCED_FACE ( 'NONE', ( #13537 ), #314, .F. ) ;
#27025 = CARTESIAN_POINT ( 'NONE',  ( -0.1968503937007874127, -0.8267716535433071723, 1.012503259137575512E-16 ) ) ;
#27026 = AXIS2_PLACEMENT_3D ( 'NONE', #24129, #546, #9141 ) ;
#27027 = AXIS2_PLACEMENT_3D ( 'NONE', #16482, #21144, #1787 ) ;
#27028 = DIRECTION ( 'NONE',  ( -0.6427876096865392519, 0.7660444431189780135, 0.000000000000000000 ) ) ;
#27029 = CARTESIAN_POINT ( 'NONE',  ( 0.03488411621188176881, 0.5314974819112028293, 1.747047244094488194 ) ) ;
#27030 = SURFACE_STYLE_FILL_AREA ( #3268 ) ;
#27031 = DIRECTION ( 'NONE',  ( 0.000000000000000000, 1.000000000000000000, 0.000000000000000000 ) ) ;
#27032 = EDGE_LOOP ( 'NONE', ( #26967, #21528, #11909, #16191 ) ) ;
#27033 = DIRECTION ( 'NONE',  ( 0.000000000000000000, 1.000000000000000000, 0.000000000000000000 ) ) ;
#27035 = DIRECTION ( 'NONE',  ( -0.2588190448135643806, 3.169619147893069890E-17, 0.9659258263664939337 ) ) ;
#27034 = AXIS2_PLACEMENT_3D ( 'NONE', #22653, #912, #5275 ) ;
#27036 = CARTESIAN_POINT ( 'NONE',  ( 0.000000000000000000, 0.6212598425196850238, -3.278217716535432842E-17 ) ) ;
#27037 = EDGE_LOOP ( 'NONE', ( #9490, #25200, #12630, #22763 ) ) ;
#27038 = DIRECTION ( 'NONE',  ( 1.000000000000000000, 0.000000000000000000, 0.000000000000000000 ) ) ;
#27039 = ORIENTED_EDGE ( 'NONE', *, *, #16585, .T. ) ;
#27040 = CARTESIAN_POINT ( 'NONE',  ( 0.4308867145619961203, -0.2480839813579571174, 0.1615162260888333701 ) ) ;
#27041 = AXIS2_PLACEMENT_3D ( 'NONE', #8769, #6381, #17526 ) ;
#27042 = DIRECTION ( 'NONE',  ( 1.000000000000000000, 0.000000000000000000, 0.000000000000000000 ) ) ;
#27043 = CARTESIAN_POINT ( 'NONE',  ( 0.1198326771653543399, 0.000000000000000000, 0.1074461786882927178 ) ) ;
#27044 = DIRECTION ( 'NONE',  ( 1.000000000000000000, 0.000000000000000000, 0.000000000000000000 ) ) ;
#27045 = LINE ( 'NONE', #1058, #14523 ) ;
#27046 = ORIENTED_EDGE ( 'NONE', *, *, #11001, .T. ) ;
#27047 = DIRECTION ( 'NONE',  ( -0.9790454724845842893, 0.1018208755700880375, -0.1763589297585410332 ) ) ;
#27048 = CARTESIAN_POINT ( 'NONE',  ( -0.09842519685039370636, 0.07874015748031495954, 0.04546065111729331171 ) ) ;
#27049 = LINE ( 'NONE', #17970, #22231 ) ;
#27050 = AXIS2_PLACEMENT_3D ( 'NONE', #15328, #17147, #25625 ) ;
#27051 = CARTESIAN_POINT ( 'NONE',  ( 0.2181198385717777743, -0.2842139414039452361, -3.115157480314960647 ) ) ;
#27052 = EDGE_LOOP ( 'NONE', ( #17219, #25964, #2641, #4080 ) ) ;
#27053 = CARTESIAN_POINT ( 'NONE',  ( 0.4218945342797225662, -0.1432577568504558585, -1.934055118110236338 ) ) ;
#27054 = CARTESIAN_POINT ( 'NONE',  ( 0.3979194638820595098, 0.2297883689023132170, -1.928289503579157183 ) ) ;
#27055 = ADVANCED_FACE ( 'NONE', ( #13271 ), #6784, .F. ) ;
#27056 = CARTESIAN_POINT ( 'NONE',  ( -0.6633461167951516524, 0.01644978644481641730, -0.2363335391394980334 ) ) ;
#27057 = ORIENTED_EDGE ( 'NONE', *, *, #901, .F. ) ;
#27058 = CARTESIAN_POINT ( 'NONE',  ( 0.09842519685039370636, 0.2165354330708661457, -3.364501312335955063 ) ) ;
#27059 = FACE_OUTER_BOUND ( 'NONE', #11389, .T. ) ;
#27060 = CARTESIAN_POINT ( 'NONE',  ( 0.4225965726692672009, 0.3242071728275124354, 1.747047244094488194 ) ) ;
#27061 = ORIENTED_EDGE ( 'NONE', *, *, #10592, .F. ) ;
#27062 = CARTESIAN_POINT ( 'NONE',  ( 0.3432721300517227458, 0.06002180498082428789, 0.1589462317926793600 ) ) ;
#27063 = AXIS2_PLACEMENT_3D ( 'NONE', #19773, #6789, #15423 ) ;
#27064 = ORIENTED_EDGE ( 'NONE', *, *, #13600, .F. ) ;
#27065 = AXIS2_PLACEMENT_3D ( 'NONE', #22186, #2810, #24845 ) ;
#27066 = CARTESIAN_POINT ( 'NONE',  ( 0.1213180142433946118, -0.3572819248074403653, -3.100567304031765392 ) ) ;
#27067 = ORIENTED_EDGE ( 'NONE', *, *, #2374, .T. ) ;
#27068 = CARTESIAN_POINT ( 'NONE',  ( -0.7874015748031496509, 0.3353269257421728211, -0.2226617707802535651 ) ) ;
#27069 = CARTESIAN_POINT ( 'NONE',  ( 0.003937007874015826907, -4.393043307086613241E-18, 0.000000000000000000 ) ) ;
#27070 = CARTESIAN_POINT ( 'NONE',  ( 0.3324885138898230341, -0.04380447413659129680, 1.953740157480315043 ) ) ;
#27071 = ORIENTED_EDGE ( 'NONE', *, *, #114, .T. ) ;
#27072 = AXIS2_PLACEMENT_3D ( 'NONE', #18058, #20358, #16267 ) ;
#27073 = CARTESIAN_POINT ( 'NONE',  ( 0.1293227632562456708, -0.3543012242648960752, 0.1992142436757342316 ) ) ;
#27074 = ORIENTED_EDGE ( 'NONE', *, *, #12850, .T. ) ;
#27075 = DIRECTION ( 'NONE',  ( 1.000000000000000000, 0.000000000000000000, 0.000000000000000000 ) ) ;
#27076 = CARTESIAN_POINT ( 'NONE',  ( 0.3996230174612964148, -0.1970259548082136380, -1.934055118110236338 ) ) ;
#27077 = VERTEX_POINT ( 'NONE', #2788 ) ;
#27078 = ORIENTED_EDGE ( 'NONE', *, *, #21633, .T. ) ;
#27079 = CARTESIAN_POINT ( 'NONE',  ( 0.3665264996331779601, -0.2116141732283464416, 0.1377952755905511861 ) ) ;
#27080 = CARTESIAN_POINT ( 'NONE',  ( 9.642888182478974314E-17, 0.07874015746264864668, 0.7874015748208159637 ) ) ;
#27081 = EDGE_CURVE ( 'NONE', #14265, #7546, #12724, .T. ) ;
#27082 = CARTESIAN_POINT ( 'NONE',  ( 0.2362439534887500470, 0.2693339498142248156, -3.115157480314960647 ) ) ;
#27083 = CYLINDRICAL_SURFACE ( 'NONE', #25654, 1.131889763779527547 ) ;
#27084 = CARTESIAN_POINT ( 'NONE',  ( 0.6055690743987126590, -0.5162970762339605946, 6.322814960629921339E-17 ) ) ;
#27085 = FACE_OUTER_BOUND ( 'NONE', #19603, .T. ) ;
#27086 = CIRCLE ( 'NONE', #25736, 0.4267795243146149664 ) ;
#27087 = DIRECTION ( 'NONE',  ( 0.000000000000000000, 0.000000000000000000, 1.000000000000000000 ) ) ;
#27088 = AXIS2_PLACEMENT_3D ( 'NONE', #22170, #26973, #7623 ) ;
#27089 = EDGE_CURVE ( 'NONE', #14598, #22705, #3402, .T. ) ;
#27090 = CARTESIAN_POINT ( 'NONE',  ( 0.3184841198566246701, -0.1570220809524502659, 1.953740157480315043 ) ) ;
#27091 = ORIENTED_EDGE ( 'NONE', *, *, #27427, .T. ) ;
#27092 = DIRECTION ( 'NONE',  ( -0.8660254037844387076, 0.4999999999999998890, 0.000000000000000000 ) ) ;
#27093 = AXIS2_PLACEMENT_3D ( 'NONE', #23998, #19633, #2373 ) ;
#27094 = DIRECTION ( 'NONE',  ( 1.000000000000000000, 0.000000000000000000, 0.000000000000000000 ) ) ;
#27095 = B_SPLINE_CURVE_WITH_KNOTS ( 'NONE', 3,
 ( #17556, #25898, #223, #21659 ),
 .UNSPECIFIED., .F., .F.,
 ( 4, 4 ),
 ( 1.219305002860847864, 1.221229623754231941 ),
 .UNSPECIFIED. ) ;
#27096 = CARTESIAN_POINT ( 'NONE',  ( -0.3265485372158890010, -0.1887320510662011952, 0.07637549214372854611 ) ) ;
#27097 = DIRECTION ( 'NONE',  ( 0.000000000000000000, 0.000000000000000000, -1.000000000000000000 ) ) ;
#27098 = CARTESIAN_POINT ( 'NONE',  ( 0.4954415918530775120, -0.1327036767659478256, 1.747047244094488194 ) ) ;
#27099 = DIMENSIONAL_EXPONENTS ( 1.000000000000000000, 0.000000000000000000, 0.000000000000000000, 0.000000000000000000, 0.000000000000000000, 0.000000000000000000, 0.000000000000000000 ) ;
#27100 = CARTESIAN_POINT ( 'NONE',  ( 0.000000000000000000, 0.000000000000000000, 0.1771653543307086520 ) ) ;
#27101 = CARTESIAN_POINT ( 'NONE',  ( 0.1649135259617042493, -0.4856708409200646281, 1.766732283464566899 ) ) ;
#27102 = VERTEX_POINT ( 'NONE', #17895 ) ;
#27103 = FACE_OUTER_BOUND ( 'NONE', #1117, .T. ) ;
#27104 = ORIENTED_EDGE ( 'NONE', *, *, #12420, .T. ) ;
#27105 = DIRECTION ( 'NONE',  ( 0.000000000000000000, 0.000000000000000000, -1.000000000000000000 ) ) ;
#27106 = ( CONVERSION_BASED_UNIT ( 'INCH', #26662 ) LENGTH_UNIT ( ) NAMED_UNIT ( #13586 ) ) ;
#27107 = CARTESIAN_POINT ( 'NONE',  ( -0.4061284506583976994, -0.2351468520617070734, 0.1992125984251968684 ) ) ;
#27108 = FACE_BOUND ( 'NONE', #19305, .T. ) ;
#27109 = ORIENTED_EDGE ( 'NONE', *, *, #4509, .F. ) ;
#27110 = ORIENTED_EDGE ( 'NONE', *, *, #4349, .T. ) ;
#27111 = EDGE_CURVE ( 'NONE', #16690, #5287, #2603, .T. ) ;
#27112 = CIRCLE ( 'NONE', #929, 0.5322834645669292097 ) ;
#27113 = CARTESIAN_POINT ( 'NONE',  ( -0.2180862235769353841, 0.4423390553432505756, -1.569881889763779625 ) ) ;
#27114 = EDGE_LOOP ( 'NONE', ( #12957, #930, #16130, #15741 ) ) ;
#27115 = FACE_OUTER_BOUND ( 'NONE', #15512, .T. ) ;
#27116 = ORIENTED_EDGE ( 'NONE', *, *, #24900, .F. ) ;
#27117 = VERTEX_POINT ( 'NONE', #5200 ) ;
#27118 = EDGE_CURVE ( 'NONE', #4089, #6287, #1051, .T. ) ;
#27119 = ITEM_DEFINED_TRANSFORMATION ( 'NONE', 'NONE', #5253,  #11588 ) ;
#27120 = CARTESIAN_POINT ( 'NONE',  ( 0.000000000000000000, 0.000000000000000000, 0.1771653543307086520 ) ) ;
#27121 = EDGE_CURVE ( 'NONE', #24230, #17929, #16786, .T. ) ;
#27122 = CARTESIAN_POINT ( 'NONE',  ( 0.5383572925355968319, -0.3100567972183901899, 0.09685039370078740717 ) ) ;
#27123 = CARTESIAN_POINT ( 'NONE',  ( -0.7434700980050996666, 0.9227202650006829376, -0.1479787484040391843 ) ) ;
#27124 = EDGE_CURVE ( 'NONE', #3293, #9025, #5638, .T. ) ;
#27125 = EDGE_CURVE ( 'NONE', #16402, #18692, #17209, .T. ) ;
#27126 = UNCERTAINTY_MEASURE_WITH_UNIT (LENGTH_MEASURE( 1.000000000000000082E-05 ), #27106, 'distance_accuracy_value', 'NONE') ;
#27127 = ORIENTED_EDGE ( 'NONE', *, *, #9851, .F. ) ;
#27128 = DIRECTION ( 'NONE',  ( 1.000000000000000000, 0.000000000000000000, 0.000000000000000000 ) ) ;
#27129 = DIRECTION ( 'NONE',  ( 0.000000000000000000, 1.000000000000000000, 0.000000000000000000 ) ) ;
#27130 = AXIS2_PLACEMENT_3D ( 'NONE', #18290, #16204, #24803 ) ;
#27131 = DIRECTION ( 'NONE',  ( 1.000000000000000000, 0.000000000000000000, 0.000000000000000000 ) ) ;
#27132 = FACE_OUTER_BOUND ( 'NONE', #14407, .T. ) ;
#27133 = DIRECTION ( 'NONE',  ( 0.000000000000000000, 0.000000000000000000, 1.000000000000000000 ) ) ;
#27134 = AXIS2_PLACEMENT_3D ( 'NONE', #13686, #566, #18181 ) ;
#27135 = AXIS2_PLACEMENT_3D ( 'NONE', #14062, #1074, #13775 ) ;
#27136 = ORIENTED_EDGE ( 'NONE', *, *, #24479, .F. ) ;
#27137 = CARTESIAN_POINT ( 'NONE',  ( 0.3214446924536846772, 0.3840069416942866742, 0.09685039370078740717 ) ) ;
#27138 = ORIENTED_EDGE ( 'NONE', *, *, #26056, .F. ) ;
#27139 = CARTESIAN_POINT ( 'NONE',  ( 1.857656692913385893E-16, 0.000000000000000000, 0.000000000000000000 ) ) ;
#27140 = ORIENTED_EDGE ( 'NONE', *, *, #23316, .T. ) ;
#27141 = CARTESIAN_POINT ( 'NONE',  ( 0.2362204724225640262, 0.000000000000000000, -4.291338582656260670 ) ) ;
#27142 = CARTESIAN_POINT ( 'NONE',  ( 0.000000000000000000, 0.1968503937007875237, -0.7874015748208159637 ) ) ;
#27143 = CARTESIAN_POINT ( 'NONE',  ( 0.04838950581350980051, 0.1968503937007873850, -3.611194239255285598 ) ) ;
#27144 = EDGE_LOOP ( 'NONE', ( #25815, #23227 ) ) ;
#27145 = ORIENTED_EDGE ( 'NONE', *, *, #19328, .F. ) ;
#27146 = EDGE_CURVE ( 'NONE', #13695, #27811, #25262, .T. ) ;
#27147 = DIRECTION ( 'NONE',  ( 0.000000000000000000, 1.000000000000000000, 0.000000000000000000 ) ) ;
#27148 = AXIS2_PLACEMENT_3D ( 'NONE', #16307, #1199, #25335 ) ;
#27149 = CARTESIAN_POINT ( 'NONE',  ( -0.0005896702191648601262, 0.4865884552430830845, 0.09284957166429641529 ) ) ;
#27150 = CARTESIAN_POINT ( 'NONE',  ( 0.000000000000000000, 0.000000000000000000, -4.209669677817527322 ) ) ;
#27151 = EDGE_CURVE ( 'NONE', #27656, #13490, #18783, .T. ) ;
#27152 = AXIS2_PLACEMENT_3D ( 'NONE', #16971, #12301, #20924 ) ;
#27153 = STYLED_ITEM ( 'NONE', ( #20525 ), #12711 ) ;
#27154 = CARTESIAN_POINT ( 'NONE',  ( -0.0005939837304750000086, 0.5007870493127504208, 0.09685039370078740717 ) ) ;
#27155 = VERTEX_POINT ( 'NONE', #27534 ) ;
#27156 = CARTESIAN_POINT ( 'NONE',  ( -0.1294857240059045234, -0.3542416573274181357, 0.07637795275590551769 ) ) ;
#27157 = EDGE_LOOP ( 'NONE', ( #12730, #24103, #13820, #9153, #24702, #1737, #22157, #10979, #14690, #8368, #10303, #8387, #12584, #690 ) ) ;
#27158 = CARTESIAN_POINT ( 'NONE',  ( 0.3324885138898233672, 0.04380447413659172701, 1.973425196850393970 ) ) ;
#27159 = CARTESIAN_POINT ( 'NONE',  ( 0.4954415918535722829, 0.1327036767636095571, -1.550196850393700920 ) ) ;
#27160 = CARTESIAN_POINT ( 'NONE',  ( -0.1293227632562458651, -0.3543012242648960752, 0.1992142436757342316 ) ) ;
#27161 = DIRECTION ( 'NONE',  ( 0.000000000000000000, 7.180547322999998243E-06, 0.9999999999742198442 ) ) ;
#27162 = CARTESIAN_POINT ( 'NONE',  ( -0.1775991818008590406, -0.5230301363771331369, 0.9202755905511811330 ) ) ;
#27163 = DIRECTION ( 'NONE',  ( 0.000000000000000000, 0.000000000000000000, -1.000000000000000000 ) ) ;
#27164 = EDGE_LOOP ( 'NONE', ( #2478, #8123 ) ) ;
#27165 = B_SPLINE_SURFACE_WITH_KNOTS ( 'NONE', 3, 3, ( 
 ( #22972, #1084, #24931, #7999, #9680 ),
 ( #7858, #1351, #22682, #16602, #3308 ),
 ( #5884, #14512, #23114, #9528, #18128 ),
 ( #26773, #11950, #18281, #7419, #16050 ) ),
 .UNSPECIFIED., .F., .F., .F.,
 ( 4, 4 ),
 ( 4, 1, 4 ),
 ( -0.5999999999999999778, 0.5999999999999999778 ),
 ( -0.003999999999996999879, 1.076708669088524140, 1.887240170904915137 ),
 .UNSPECIFIED. ) ;
#27166 = DIRECTION ( 'NONE',  ( -1.000000000000000000, 0.000000000000000000, 0.000000000000000000 ) ) ;
#27167 = DIRECTION ( 'NONE',  ( 8.659560554583420347E-17, -0.7071067818211396183, 0.7071067805519553051 ) ) ;
#27168 = VERTEX_POINT ( 'NONE', #8178 ) ;
#27169 = B_SPLINE_CURVE_WITH_KNOTS ( 'NONE', 3,
 ( #21985, #24925, #27062, #9523, #13491, #18120 ),
 .UNSPECIFIED., .F., .F.,
 ( 4, 2, 4 ),
 ( 0.5000000000000000000, 0.7500000000000000000, 1.000000000000000000 ),
 .UNSPECIFIED. ) ;
#27170 = DIRECTION ( 'NONE',  ( 1.000000000000000000, 0.000000000000000000, 0.000000000000000000 ) ) ;
#27171 = CARTESIAN_POINT ( 'NONE',  ( 0.3242892624569754800, 0.4225434286518392479, 1.747047244094487972 ) ) ;
#27172 = ORIENTED_EDGE ( 'NONE', *, *, #16269, .F. ) ;
#27173 = CIRCLE ( 'NONE', #21332, 0.1023622047244094474 ) ;
#27174 = ORIENTED_EDGE ( 'NONE', *, *, #27758, .T. ) ;
#27175 = DIRECTION ( 'NONE',  ( 0.3832738344365670957, 0.9236347588935202024, 0.000000000000000000 ) ) ;
#27176 = DIRECTION ( 'NONE',  ( -1.000000000000000000, 0.000000000000000000, 0.000000000000000000 ) ) ;
#27177 = DIRECTION ( 'NONE',  ( 0.000000000000000000, 0.000000000000000000, 1.000000000000000000 ) ) ;
#27178 = CARTESIAN_POINT ( 'NONE',  ( 0.3976891862754212137, 1.133679329692560245, -0.4395307839725697274 ) ) ;
#27179 = EDGE_LOOP ( 'NONE', ( #27071, #1636, #8822, #23635 ) ) ;
#27180 = ORIENTED_EDGE ( 'NONE', *, *, #12351, .T. ) ;
#27181 = EDGE_CURVE ( 'NONE', #11007, #15797, #12958, .T. ) ;
#27182 = CARTESIAN_POINT ( 'NONE',  ( -0.4216927985367120990, -0.2427835582309759432, 0.1827409795191895503 ) ) ;
#27183 = CARTESIAN_POINT ( 'NONE',  ( -0.1718374205099799101, -0.4703827404237102550, 0.2574803149606298969 ) ) ;
#27184 = DIRECTION ( 'NONE',  ( -1.000000000000000000, 0.000000000000000000, 0.000000000000000000 ) ) ;
#27185 = DIRECTION ( 'NONE',  ( 0.9790454724845839563, 0.1018208755700887314, -0.1763589297585421989 ) ) ;
#27186 = CARTESIAN_POINT ( 'NONE',  ( -0.8031496062992127261, 9.835745945907876618E-17, 0.02362204724409448786 ) ) ;
#27187 = CARTESIAN_POINT ( 'NONE',  ( 0.4898768902087983768, -1.356024015748031595E-16, -0.2362204724409449064 ) ) ;
#27188 = EDGE_CURVE ( 'NONE', #22411, #14218, #26921, .T. ) ;
#27189 = TOROIDAL_SURFACE ( 'NONE', #8232, 0.3031496062992122820, 0.01181102362204755792 ) ;
#27190 = CARTESIAN_POINT ( 'NONE',  ( -0.2118615749922468650, -0.5840192333899535404, 0.2574803149606298969 ) ) ;
#27191 = CARTESIAN_POINT ( 'NONE',  ( -0.4684132450478834531, -0.1062614382955279352, 0.2194422276446760245 ) ) ;
#27192 = AXIS2_PLACEMENT_3D ( 'NONE', #26531, #22172, #24287 ) ;
#27193 = CARTESIAN_POINT ( 'NONE',  ( 0.1490609433494345937, 0.4786070381568061638, 0.004730797288071140853 ) ) ;
#27194 = CARTESIAN_POINT ( 'NONE',  ( -0.1151343661285636755, -0.3392608232660268563, -3.115157480314960647 ) ) ;
#27195 = VERTEX_POINT ( 'NONE', #10421 ) ;
#27196 = CARTESIAN_POINT ( 'NONE',  ( -0.02909913904662089768, -0.4446020952038907681, -1.934055118110236338 ) ) ;
#27197 = AXIS2_PLACEMENT_3D ( 'NONE', #19547, #231, #11197 ) ;
#27198 = ADVANCED_FACE ( 'NONE', ( #25550 ), #22859, .T. ) ;
#27199 = CARTESIAN_POINT ( 'NONE',  ( -0.4473595089310440920, -0.7616466953483976843, -0.01204780428933531489 ) ) ;
#27200 = CARTESIAN_POINT ( 'NONE',  ( -0.3512268162760395773, 0.4004221243553298115, 1.747047244094488194 ) ) ;
#27201 = ORIENTED_EDGE ( 'NONE', *, *, #10554, .T. ) ;
#27202 = ( LENGTH_UNIT ( ) NAMED_UNIT ( * ) SI_UNIT ( $, .METRE. ) ) ;
#27203 = AXIS2_PLACEMENT_3D ( 'NONE', #11211, #2588, #15610 ) ;
#27204 = ORIENTED_EDGE ( 'NONE', *, *, #21337, .T. ) ;
#27205 = ORIENTED_EDGE ( 'NONE', *, *, #22244, .T. ) ;
#27206 = CARTESIAN_POINT ( 'NONE',  ( -0.2488091035917009419, 0.2836590635674538508, -3.100567304031763172 ) ) ;
#27207 = CARTESIAN_POINT ( 'NONE',  ( 0.2078289949484099508, -0.4330237525398077936, 0.2362204724409449619 ) ) ;
#27208 = CARTESIAN_POINT ( 'NONE',  ( -0.3584231247409862542, 0.000000000000000000, -0.04133858267716535029 ) ) ;
#27209 = ORIENTED_EDGE ( 'NONE', *, *, #19159, .F. ) ;
#27210 = DIRECTION ( 'NONE',  ( 0.000000000000000000, 0.000000000000000000, -1.000000000000000000 ) ) ;
#27211 = DIRECTION ( 'NONE',  ( 0.000000000000000000, -1.000000000000000000, 0.000000000000000000 ) ) ;
#27212 = ORIENTED_EDGE ( 'NONE', *, *, #2720, .T. ) ;
#27213 = ORIENTED_EDGE ( 'NONE', *, *, #14708, .T. ) ;
#27214 = CARTESIAN_POINT ( 'NONE',  ( 0.000000000000000000, 0.5322834645669292097, 0.3401599409343964431 ) ) ;
#27215 = DIRECTION ( 'NONE',  ( 0.3420201433256691570, -0.9396926207859082059, 0.000000000000000000 ) ) ;
#27216 = EDGE_CURVE ( 'NONE', #4089, #14153, #1949, .T. ) ;
#27217 = EDGE_CURVE ( 'NONE', #1802, #26980, #18112, .T. ) ;
#27218 = CARTESIAN_POINT ( 'NONE',  ( 0.02339816079119036787, -0.3574975638436101444, -3.115157480314960647 ) ) ;
#27219 = CARTESIAN_POINT ( 'NONE',  ( 0.000000000000000000, 0.000000000000000000, -0.2755905511811023723 ) ) ;
#27220 = CARTESIAN_POINT ( 'NONE',  ( -0.3346456692913387099, 0.04380501567505452193, 1.973425196850393970 ) ) ;
#27221 = CARTESIAN_POINT ( 'NONE',  ( -0.3040421205569480145, 1.096420371425407492, -0.7554543140018661340 ) ) ;
#27222 = TOROIDAL_SURFACE ( 'NONE', #14602, 0.3031496062992122820, 0.01181102362204755792 ) ;
#27223 = PLANE ( 'NONE',  #21311 ) ;
#27224 = CONICAL_SURFACE ( 'NONE', #20910, 0.4537419570391968415, 1.365720138124999927 ) ;
#27225 = FACE_OUTER_BOUND ( 'NONE', #11658, .T. ) ;
#27226 = CARTESIAN_POINT ( 'NONE',  ( 0.3332647802741406373, 4.241214765863767561E-17, -0.1692378991623492424 ) ) ;
#27227 = AXIS2_PLACEMENT_3D ( 'NONE', #10000, #22869, #12120 ) ;
#27228 = EDGE_LOOP ( 'NONE', ( #23777, #23722 ) ) ;
#27229 = CARTESIAN_POINT ( 'NONE',  ( 0.5672055940108537975, 0.07462095020313340432, 0.9399606299212600602 ) ) ;
#27230 = AXIS2_PLACEMENT_3D ( 'NONE', #6083, #12696, #10290 ) ;
#27231 = DIRECTION ( 'NONE',  ( 0.000000000000000000, 0.000000000000000000, 1.000000000000000000 ) ) ;
#27232 = CARTESIAN_POINT ( 'NONE',  ( -0.3264619303874877754, -0.1888818218344748001, 0.07637630750536809898 ) ) ;
#27233 = AXIS2_PLACEMENT_3D ( 'NONE', #13250, #17491, #23991 ) ;
#27234 = DIRECTION ( 'NONE',  ( 0.000000000000000000, 0.000000000000000000, 1.000000000000000000 ) ) ;
#27235 = CARTESIAN_POINT ( 'NONE',  ( 0.03478633594543814600, -0.5314960629921260393, 1.747047244094488194 ) ) ;
#27236 = CARTESIAN_POINT ( 'NONE',  ( -0.06699507805368211388, 0.5085118447801414421, 1.747047244094488194 ) ) ;
#27237 = ORIENTED_EDGE ( 'NONE', *, *, #14761, .F. ) ;
#27238 = VECTOR ( 'NONE', #947, 39.37007874015748143 ) ;
#27239 = EDGE_CURVE ( 'NONE', #8846, #2394, #8040, .T. ) ;
#27240 = EDGE_LOOP ( 'NONE', ( #15897, #11253 ) ) ;
#27241 = CARTESIAN_POINT ( 'NONE',  ( 0.5905511811023621549, 4.580371886574746102E-17, 0.3740157480314960647 ) ) ;
#27242 = ORIENTED_EDGE ( 'NONE', *, *, #9660, .F. ) ;
#27243 = FACE_OUTER_BOUND ( 'NONE', #22303, .T. ) ;
#27244 = CARTESIAN_POINT ( 'NONE',  ( -0.3349573549949658169, 0.2938049579018958690, -1.934055118110236338 ) ) ;
#27245 = CARTESIAN_POINT ( 'NONE',  ( 0.1493295869868995207, -0.4796200322302701657, 0.01881014177837847870 ) ) ;
#27246 = B_SPLINE_CURVE_WITH_KNOTS ( 'NONE', 3,
 ( #8617, #16828, #19354, #21343, #6649, #8756, #12989, #19488, #15275, #15136, #23747 ),
 .UNSPECIFIED., .F., .F.,
 ( 4, 2, 1, 2, 2, 4 ),
 ( 0.000000000000000000, 0.1249999999999981681, 0.1874999999999971689, 0.2187499999999970024, 0.2499999999999968359, 0.5000000000000000000 ),
 .UNSPECIFIED. ) ;
#27247 = VECTOR ( 'NONE', #17823, 39.37007874015748854 ) ;
#27248 = CARTESIAN_POINT ( 'NONE',  ( 0.6299212598425196763, 0.07910393700787400617, 1.087052427555504903E-17 ) ) ;
#27249 = VERTEX_POINT ( 'NONE', #11119 ) ;
#27250 = VERTEX_POINT ( 'NONE', #2630 ) ;
#27251 = CARTESIAN_POINT ( 'NONE',  ( -0.06441834428466812479, 0.4889536969035060410, -1.550196850393700920 ) ) ;
#27252 = EDGE_CURVE ( 'NONE', #7492, #22807, #23410, .T. ) ;
#27253 = ORIENTED_EDGE ( 'NONE', *, *, #1444, .T. ) ;
#27254 = ORIENTED_EDGE ( 'NONE', *, *, #8957, .T. ) ;
#27255 = CIRCLE ( 'NONE', #15086, 0.5511811023622047445 ) ;
#27256 = VECTOR ( 'NONE', #23325, 39.37007874015748143 ) ;
#27257 = FACE_BOUND ( 'NONE', #1410, .T. ) ;
#27258 = ORIENTED_EDGE ( 'NONE', *, *, #14714, .T. ) ;
#27259 = CIRCLE ( 'NONE', #10555, 0.3722026523000413478 ) ;
#27260 = DIRECTION ( 'NONE',  ( 0.000000000000000000, 0.000000000000000000, -1.000000000000000000 ) ) ;
#27261 = DIRECTION ( 'NONE',  ( 0.000000000000000000, 1.000000000000000000, 0.000000000000000000 ) ) ;
#27262 = CARTESIAN_POINT ( 'NONE',  ( -0.5638041354701026631, -0.3277633461629020917, 0.1938474616169392761 ) ) ;
#27263 = CARTESIAN_POINT ( 'NONE',  ( -0.06200787401574805319, 0.000000000000000000, -4.015748031496062964 ) ) ;
#27264 = CARTESIAN_POINT ( 'NONE',  ( -0.7165354330708662012, 8.847349907225958695E-17, -3.278217716535432842E-17 ) ) ;
#27265 = ADVANCED_FACE ( 'NONE', ( #17038 ), #18716, .F. ) ;
#27266 = CIRCLE ( 'NONE', #6984, 0.07874015748031489015 ) ;
#27267 = EDGE_LOOP ( 'NONE', ( #11703, #6735 ) ) ;
#27268 = AXIS2_PLACEMENT_3D ( 'NONE', #24452, #5103, #13728 ) ;
#27269 = ORIENTED_EDGE ( 'NONE', *, *, #13804, .T. ) ;
#27270 = EDGE_CURVE ( 'NONE', #6364, #1472, #19243, .T. ) ;
#27271 = ORIENTED_EDGE ( 'NONE', *, *, #7627, .F. ) ;
#27272 = CARTESIAN_POINT ( 'NONE',  ( -0.2564944395535628252, -0.4441657790094413749, -1.550196850393700920 ) ) ;
#27273 = DIRECTION ( 'NONE',  ( 0.000000000000000000, 0.000000000000000000, 1.000000000000000000 ) ) ;
#27274 = EDGE_CURVE ( 'NONE', #17602, #19029, #1655, .T. ) ;
#27275 = CARTESIAN_POINT ( 'NONE',  ( 0.2952755905264887182, 0.000000000000000000, -4.330708661417323135 ) ) ;
#27276 = CARTESIAN_POINT ( 'NONE',  ( -6.518592411209533944E-17, -0.5322834645669292097, 0.4724409448818898127 ) ) ;
#27277 = DIMENSIONAL_EXPONENTS ( 1.000000000000000000, 0.000000000000000000, 0.000000000000000000, 0.000000000000000000, 0.000000000000000000, 0.000000000000000000, 0.000000000000000000 ) ;
#27278 = ORIENTED_EDGE ( 'NONE', *, *, #2713, .F. ) ;
#27279 = CARTESIAN_POINT ( 'NONE',  ( -0.3713448905834433322, 0.06600512665679449109, 0.1992125984251968684 ) ) ;
#27280 = VECTOR ( 'NONE', #821, 39.37007874015748143 ) ;
#27281 = CARTESIAN_POINT ( 'NONE',  ( -0.3937007874015748254, 0.000000000000000000, -0.07578740157480315376 ) ) ;
#27282 = ORIENTED_EDGE ( 'NONE', *, *, #24972, .F. ) ;
#27283 = DIRECTION ( 'NONE',  ( 1.000000000000000000, 0.000000000000000000, 0.000000000000000000 ) ) ;
#27284 = CARTESIAN_POINT ( 'NONE',  ( 0.3263749705684267921, -0.1890319631540330891, 0.1992125984251968684 ) ) ;
#27285 = VECTOR ( 'NONE', #25141, 39.37007874015748854 ) ;
#27286 = CARTESIAN_POINT ( 'NONE',  ( -0.1718374205099799101, -0.4703827404237102550, 0.2574803149606298969 ) ) ;
#27287 = DIRECTION ( 'NONE',  ( 0.1736481776669313026, 0.9848077530122077983, 0.000000000000000000 ) ) ;
#27288 = AXIS2_PLACEMENT_3D ( 'NONE', #24878, #22914, #25306 ) ;
#27289 = ORIENTED_EDGE ( 'NONE', *, *, #18973, .F. ) ;
#27290 = EDGE_LOOP ( 'NONE', ( #20444, #20630, #15421 ) ) ;
#27291 = FACE_OUTER_BOUND ( 'NONE', #9387, .T. ) ;
#27292 = CARTESIAN_POINT ( 'NONE',  ( 0.3239425792934479409, 0.08676778863010962961, 1.953740157480315043 ) ) ;
#27293 = CARTESIAN_POINT ( 'NONE',  ( 0.000000000000000000, 0.000000000000000000, 0.3401574803149606252 ) ) ;
#27294 = EDGE_CURVE ( 'NONE', #6009, #13528, #11717, .T. ) ;
#27295 = CARTESIAN_POINT ( 'NONE',  ( 0.4152525734086595088, -0.3642352168757885811, 0.9399606299212598381 ) ) ;
#27296 = CARTESIAN_POINT ( 'NONE',  ( -0.1189624676717062762, -0.3253923344978156829, 0.1478915661218652144 ) ) ;
#27297 = ORIENTED_EDGE ( 'NONE', *, *, #17648, .T. ) ;
#27298 = CARTESIAN_POINT ( 'NONE',  ( -0.2313498293151122209, -0.4793777142568558802, 0.3401591244667909186 ) ) ;
#27299 = CONICAL_SURFACE ( 'NONE', #21877, 0.2952755905511805778, 0.2617993875000016457 ) ;
#27300 = EDGE_CURVE ( 'NONE', #1935, #25537, #25220, .T. ) ;
#27301 = DIRECTION ( 'NONE',  ( 0.000000000000000000, 0.000000000000000000, 1.000000000000000000 ) ) ;
#27302 = VERTEX_POINT ( 'NONE', #19286 ) ;
#27303 = ( REPRESENTATION_RELATIONSHIP ('NONE','NONE', #12434, #16232 ) REPRESENTATION_RELATIONSHIP_WITH_TRANSFORMATION ( #21318 )SHAPE_REPRESENTATION_RELATIONSHIP( ) ) ;
#27304 = CARTESIAN_POINT ( 'NONE',  ( 0.000000000000000000, 0.6102362204724409711, 0.2362204724409449064 ) ) ;
#27305 = ADVANCED_FACE ( 'NONE', ( #16750 ), #337, .F. ) ;
#27306 = VERTEX_POINT ( 'NONE', #13069 ) ;
#27307 = AXIS2_PLACEMENT_3D ( 'NONE', #26155, #11436, #712 ) ;
#27308 = DIRECTION ( 'NONE',  ( -0.5000000000000061062, 0.000000000000000000, 0.8660254037844351549 ) ) ;
#27309 = CIRCLE ( 'NONE', #18265, 0.4786070381542913421 ) ;
#27310 = CARTESIAN_POINT ( 'NONE',  ( 0.3339160553493882300, 1.214868409966151530, -0.6104964979807637748 ) ) ;
#27311 = DIRECTION ( 'NONE',  ( -1.000000000000000000, 0.000000000000000000, 0.000000000000000000 ) ) ;
#27312 = DIRECTION ( 'NONE',  ( -0.000000000000000000, -0.000000000000000000, -1.000000000000000000 ) ) ;
#27313 = ORIENTED_EDGE ( 'NONE', *, *, #24079, .F. ) ;
#27314 = CARTESIAN_POINT ( 'NONE',  ( 0.03532354024591712049, -0.8267716535433070613, 0.8267716535433071723 ) ) ;
#27315 = ORIENTED_EDGE ( 'NONE', *, *, #383, .T. ) ;
#27316 = CARTESIAN_POINT ( 'NONE',  ( 0.2236164729194649314, 0.2672714825446357856, 0.1166443193927515082 ) ) ;
#27317 = CARTESIAN_POINT ( 'NONE',  ( 1.197070535079588716, 0.07874015748031495954, -1.078960298859116707 ) ) ;
#27318 = CARTESIAN_POINT ( 'NONE',  ( -0.09842519685039373412, 0.2991866959364303802, -3.272637795275590733 ) ) ;
#27319 = CARTESIAN_POINT ( 'NONE',  ( 1.197070535079588716, 0.4724409448818898127, 1.315180771300060503 ) ) ;
#27320 = CARTESIAN_POINT ( 'NONE',  ( -0.3412792617076849111, 0.05967164814832635888, 0.1377952755905512139 ) ) ;
#27321 = CARTESIAN_POINT ( 'NONE',  ( 0.1490609433576163545, 0.2393035190829114200, 0.4144858534816307505 ) ) ;
#27322 = ORIENTED_EDGE ( 'NONE', *, *, #19106, .F. ) ;
#27323 = CONICAL_SURFACE ( 'NONE', #25977, 0.1318897637674583401, 0.5235987755982981495 ) ;
#27324 = ADVANCED_FACE ( 'NONE', ( #24216 ), #5722, .F. ) ;
#27325 = CARTESIAN_POINT ( 'NONE',  ( 0.4692913385826771866, 0.000000000000000000, 0.1992125984251968684 ) ) ;
#27326 = CARTESIAN_POINT ( 'NONE',  ( 0.1520643344662694629, 0.4930463976998556985, -0.03726710077533019333 ) ) ;
#27327 = CARTESIAN_POINT ( 'NONE',  ( 0.1522836969735573143, 0.4909267390297480382, 0.05591742528025173131 ) ) ;
#27328 = ORIENTED_EDGE ( 'NONE', *, *, #10508, .F. ) ;
#27329 = VERTEX_POINT ( 'NONE', #21828 ) ;
#27330 = CARTESIAN_POINT ( 'NONE',  ( 0.1432577568504648236, 0.4218945342797248421, -1.934055118110236338 ) ) ;
#27331 = AXIS2_PLACEMENT_3D ( 'NONE', #26291, #6953, #15575 ) ;
#27332 = ADVANCED_FACE ( 'NONE', ( #2320 ), #376, .F. ) ;
#27333 = AXIS2_PLACEMENT_3D ( 'NONE', #14930, #27627, #7857 ) ;
#27334 = VERTEX_POINT ( 'NONE', #15747 ) ;
#27335 = EDGE_CURVE ( 'NONE', #22723, #17590, #8417, .T. ) ;
#27336 = VERTEX_POINT ( 'NONE', #4854 ) ;
#27337 = CARTESIAN_POINT ( 'NONE',  ( -0.3338887748335570560, -1.269220122646561144, -0.8285976369166339062 ) ) ;
#27338 = APPLICATION_PROTOCOL_DEFINITION ( 'draft international standard', 'automotive_design', 1998, #2576 ) ;
#27339 = CARTESIAN_POINT ( 'NONE',  ( 0.2663596103035608120, 0.4612490782035171266, 1.747047244094488194 ) ) ;
#27340 = EDGE_CURVE ( 'NONE', #14847, #4552, #7064, .T. ) ;
#27341 = AXIS2_PLACEMENT_3D ( 'NONE', #25381, #12390, #25667 ) ;
#27342 = PRESENTATION_STYLE_ASSIGNMENT (( #20700 ) ) ;
#27343 = ORIENTED_EDGE ( 'NONE', *, *, #23601, .F. ) ;
#27344 = CARTESIAN_POINT ( 'NONE',  ( -0.3740848232703753440, -0.04928467685643751067, -3.100567304031760507 ) ) ;
#27345 = FACE_OUTER_BOUND ( 'NONE', #24978, .T. ) ;
#27346 = CARTESIAN_POINT ( 'NONE',  ( 0.1287090038540880110, 0.000000000000000000, 0.1968503937007874127 ) ) ;
#27347 = EDGE_CURVE ( 'NONE', #11692, #26228, #11077, .T. ) ;
#27348 = B_SPLINE_CURVE_WITH_KNOTS ( 'NONE', 3,
 ( #3040, #9542, #5468, #18145, #9837, #16347, #20718, #1364, #9976, #26789, #26940, #16066, #11818, #16479, #18576, #22557, #27220, #1099 ),
 .UNSPECIFIED., .F., .F.,
 ( 4, 2, 2, 2, 2, 2, 2, 2, 4 ),
 ( 0.000000000000000000, 0.06249999999999997224, 0.1249999999999999722, 0.1874999999999999722, 0.2499999999999999445, 0.3124999999999999445, 0.3750000000000000000, 0.4375000000000000000, 0.5000000000000000000 ),
 .UNSPECIFIED. ) ;
#27349 = CARTESIAN_POINT ( 'NONE',  ( 0.3543307086614173596, 0.02319089060379041917, 1.953740157480315043 ) ) ;
#27350 = ORIENTED_EDGE ( 'NONE', *, *, #10208, .F. ) ;
#27351 = CARTESIAN_POINT ( 'NONE',  ( -0.5145594007491112176, -0.3210976060043693181, -0.3019172820411493707 ) ) ;
#27352 = CARTESIAN_POINT ( 'NONE',  ( -0.5724622793729822190, -0.3313001865996386686, 0.1616495878883337511 ) ) ;
#27354 = CARTESIAN_POINT ( 'NONE',  ( 0.1839420097223146422, 0.5417097841049177687, 0.9399606299212598381 ) ) ;
#27353 = CARTESIAN_POINT ( 'NONE',  ( -0.3667122560601320802, -0.09855118063547678442, -3.100567304031763172 ) ) ;
#27355 = CIRCLE ( 'NONE', #4768, 0.5393700787401575214 ) ;
#27356 = DIRECTION ( 'NONE',  ( 0.000000000000000000, 0.000000000000000000, -1.000000000000000000 ) ) ;
#27357 = EDGE_LOOP ( 'NONE', ( #4520, #3731, #17106, #22724, #14216 ) ) ;
#27358 = EDGE_LOOP ( 'NONE', ( #19097, #2892, #16189, #25533 ) ) ;
#27359 = CARTESIAN_POINT ( 'NONE',  ( 0.000000000000000000, 0.1968503937007874127, 0.000000000000000000 ) ) ;
#27360 = CYLINDRICAL_SURFACE ( 'NONE', #11763, 0.06200787401574805319 ) ;
#27361 = CARTESIAN_POINT ( 'NONE',  ( -0.3574975638436101444, -0.02339816079122979120, -3.115157480314960647 ) ) ;
#27362 = CARTESIAN_POINT ( 'NONE',  ( 0.1516263115863346334, 0.1971492568089275588, 0.4530651079966787620 ) ) ;
#27363 = FACE_BOUND ( 'NONE', #12148, .T. ) ;
#27364 = CARTESIAN_POINT ( 'NONE',  ( 6.026805113914139867E-17, 0.9055118110236221041, 0.4921259842519685179 ) ) ;
#27365 = CARTESIAN_POINT ( 'NONE',  ( 0.000000000000000000, 0.000000000000000000, 2.504921259842519898 ) ) ;
#27366 = CARTESIAN_POINT ( 'NONE',  ( -0.1968503937007874127, -1.381459842519685169E-18, 0.09092130223458683158 ) ) ;
#27367 = CARTESIAN_POINT ( 'NONE',  ( 0.000000000000000000, 0.000000000000000000, -0.2204724409448818867 ) ) ;
#27368 = DIRECTION ( 'NONE',  ( -1.000000000000000000, 0.000000000000000000, 0.000000000000000000 ) ) ;
#27369 = VERTEX_POINT ( 'NONE', #254 ) ;
#27370 = CARTESIAN_POINT ( 'NONE',  ( 0.1136811023622047168, 0.000000000000000000, 0.000000000000000000 ) ) ;
#27371 = EDGE_CURVE ( 'NONE', #22748, #20633, #13468, .T. ) ;
#27372 = CARTESIAN_POINT ( 'NONE',  ( -0.2602238532265429005, 0.000000000000000000, -0.2362204724409449064 ) ) ;
#27373 = DIRECTION ( 'NONE',  ( 1.000000000000000000, 0.000000000000000000, 0.000000000000000000 ) ) ;
#27374 = FACE_OUTER_BOUND ( 'NONE', #16640, .T. ) ;
#27375 = CARTESIAN_POINT ( 'NONE',  ( 0.3223547283257516272, 0.3832433309296771617, 0.2574803149606298969 ) ) ;
#27376 = CARTESIAN_POINT ( 'NONE',  ( 0.1259842519685039353, 0.000000000000000000, 0.000000000000000000 ) ) ;
#27377 = CARTESIAN_POINT ( 'NONE',  ( 6.136516277395897527E-17, 0.2165354330708661457, -3.646653543307086576 ) ) ;
#27378 = ADVANCED_FACE ( 'NONE', ( #13198, #15204 ), #8955, .T. ) ;
#27379 = CARTESIAN_POINT ( 'NONE',  ( -0.5085118447801421082, 0.06699507805369804558, 1.766732283464566899 ) ) ;
#27380 = ORIENTED_EDGE ( 'NONE', *, *, #12647, .F. ) ;
#27381 = EDGE_CURVE ( 'NONE', #12564, #17190, #19709, .T. ) ;
#27382 = EDGE_LOOP ( 'NONE', ( #26233, #24247, #25639, #19570, #25433, #908, #17803, #12464, #12069, #1878, #22026 ) ) ;
#27383 = CARTESIAN_POINT ( 'NONE',  ( -0.3551931031211768008, 0.04679574315772456333, -3.115157480314960647 ) ) ;
#27384 = VERTEX_POINT ( 'NONE', #26332 ) ;
#27385 = CARTESIAN_POINT ( 'NONE',  ( 0.4535326485287339282, 0.08054850140356757671, 0.1771653543307084855 ) ) ;
#27386 = SHAPE_REPRESENTATION_RELATIONSHIP ( 'NONE' , 'NONE' ,  #16232, #23850 ) ;
#27387 = CARTESIAN_POINT ( 'NONE',  ( -0.0005056364805145227657, 0.3583524373837457255, 0.09506557084337692587 ) ) ;
#27388 = CARTESIAN_POINT ( 'NONE',  ( 0.3346456692913385988, 0.000000000000000000, 1.953740157480315043 ) ) ;
#27389 = EDGE_LOOP ( 'NONE', ( #14794, #15142, #17098, #3745, #5447, #9568, #23975 ) ) ;
#27390 = ORIENTED_EDGE ( 'NONE', *, *, #705, .T. ) ;
#27391 = CARTESIAN_POINT ( 'NONE',  ( 0.4889536969034951053, 0.06441834428467130280, -1.550196850393700920 ) ) ;
#27392 = ORIENTED_EDGE ( 'NONE', *, *, #4810, .T. ) ;
#27393 = VERTEX_POINT ( 'NONE', #6855 ) ;
#27394 = EDGE_LOOP ( 'NONE', ( #14764, #27849, #16590, #19333 ) ) ;
#27395 = B_SPLINE_CURVE_WITH_KNOTS ( 'NONE', 3,
 ( #16660, #12270, #14416, #1393, #19044, #21031 ),
 .UNSPECIFIED., .F., .F.,
 ( 4, 2, 4 ),
 ( 0.3108507187342960387, 0.3125269569790670166, 0.3142031952238389936 ),
 .UNSPECIFIED. ) ;
#27396 = CONTEXT_DEPENDENT_SHAPE_REPRESENTATION ( #20448, #22223 ) ;
#27397 = CIRCLE ( 'NONE', #2124, 0.3937007874015748254 ) ;
#27398 = CARTESIAN_POINT ( 'NONE',  ( -0.3765118517642104257, 2.305470170520414967E-17, -3.100567304031763172 ) ) ;
#27399 = DIRECTION ( 'NONE',  ( 0.000000000000000000, 1.000000000000000000, 0.000000000000000000 ) ) ;
#27400 = LINE ( 'NONE', #11851, #26268 ) ;
#27401 = CARTESIAN_POINT ( 'NONE',  ( -0.4333973147258542991, -0.2509079296564011852, 0.2574803149606298969 ) ) ;
#27402 = PRODUCT ( 'Deep Groove Ball Bearing 15x28x7', 'Deep Groove Ball Bearing 15x28x7', '', ( #8842 ) ) ;
#27403 = ORIENTED_EDGE ( 'NONE', *, *, #8868, .T. ) ;
#27404 = CARTESIAN_POINT ( 'NONE',  ( -1.928577543407793639E-16, 0.4724409448818898127, 1.811023622047243542 ) ) ;
#27405 = DIRECTION ( 'NONE',  ( 1.000000000000000000, 0.000000000000000000, 0.000000000000000000 ) ) ;
#27406 = DIRECTION ( 'NONE',  ( 0.000000000000000000, 0.000000000000000000, 1.000000000000000000 ) ) ;
#27407 = DIRECTION ( 'NONE',  ( 0.000000000000000000, 0.000000000000000000, -1.000000000000000000 ) ) ;
#27408 = DIRECTION ( 'NONE',  ( 0.000000000000000000, -1.000000000000000000, 0.000000000000000000 ) ) ;
#27409 = EDGE_CURVE ( 'NONE', #8587, #17370, #8690, .T. ) ;
#27410 = ORIENTED_EDGE ( 'NONE', *, *, #5649, .T. ) ;
#27411 = AXIS2_PLACEMENT_3D ( 'NONE', #20944, #12048, #16711 ) ;
#27412 = CARTESIAN_POINT ( 'NONE',  ( 0.1522836969815822838, -0.2938892803218252081, 0.3971963147669425598 ) ) ;
#27413 = ORIENTED_EDGE ( 'NONE', *, *, #21126, .F. ) ;
#27414 = AXIS2_PLACEMENT_3D ( 'NONE', #15488, #13909, #7130 ) ;
#27415 = CARTESIAN_POINT ( 'NONE',  ( 0.1294857240059045234, -0.3542416573274181357, 0.07637795275590551769 ) ) ;
#27416 = ORIENTED_EDGE ( 'NONE', *, *, #1786, .T. ) ;
#27417 = CIRCLE ( 'NONE', #15256, 0.8267716535433071723 ) ;
#27418 = DIRECTION ( 'NONE',  ( -0.3420201433256691570, 0.9396926207859084279, 0.000000000000000000 ) ) ;
#27419 = CARTESIAN_POINT ( 'NONE',  ( 0.6791338582677166613, -0.5893189861902062843, -8.232839077402887083E-17 ) ) ;
#27420 = ORIENTED_EDGE ( 'NONE', *, *, #10264, .T. ) ;
#27421 = CYLINDRICAL_SURFACE ( 'NONE', #9982, 0.3722026523000413478 ) ;
#27422 = EDGE_LOOP ( 'NONE', ( #14664, #11762, #18381, #12557 ) ) ;
#27423 = CARTESIAN_POINT ( 'NONE',  ( -0.2243259791915123424, -0.6183223858009434526, 0.2081850588310771299 ) ) ;
#27424 = CARTESIAN_POINT ( 'NONE',  ( -1.197070535079588716, 0.4724409448818898127, 1.315180771300060503 ) ) ;
#27425 = DIRECTION ( 'NONE',  ( 1.000000000000000000, 0.000000000000000000, 0.000000000000000000 ) ) ;
#27426 = EDGE_CURVE ( 'NONE', #13098, #15615, #304, .T. ) ;
#27427 = EDGE_CURVE ( 'NONE', #12947, #280, #25580, .T. ) ;
#27428 = CARTESIAN_POINT ( 'NONE',  ( -0.09586345222256538456, 0.2165354330708661457, -3.573990933995853769 ) ) ;
#27429 = ORIENTED_EDGE ( 'NONE', *, *, #5259, .F. ) ;
#27430 = CARTESIAN_POINT ( 'NONE',  ( -0.1570092758121683085, -0.4330450457732859526, 0.1639447408239428638 ) ) ;
#27431 = AXIS2_PLACEMENT_3D ( 'NONE', #3424, #24352, #5281 ) ;
#27432 = CARTESIAN_POINT ( 'NONE',  ( 0.3324885138898166503, 0.04380447413659039474, 1.953740157480315043 ) ) ;
#27433 = CARTESIAN_POINT ( 'NONE',  ( 0.1649135259639267770, -0.4856708409191258236, -1.550196850393700920 ) ) ;
#27434 = ADVANCED_FACE ( 'NONE', ( #2462 ), #6994, .F. ) ;
#27436 = CARTESIAN_POINT ( 'NONE',  ( -0.2762247810519084523, -0.4783323773986298266, 0.9399606299212598381 ) ) ;
#27435 = CIRCLE ( 'NONE', #20205, 0.5511811023975373702 ) ;
#27437 = ADVANCED_FACE ( 'NONE', ( #11217, #1055 ), #14046, .T. ) ;
#27438 = EDGE_CURVE ( 'NONE', #10695, #12956, #9796, .T. ) ;
#27439 = VECTOR ( 'NONE', #19063, 39.37007874015748143 ) ;
#27440 = CARTESIAN_POINT ( 'NONE',  ( -0.2362204724409449064, 0.9448818897637796255, -9.561468503937007847E-18 ) ) ;
#27441 = ORIENTED_EDGE ( 'NONE', *, *, #12347, .T. ) ;
#27442 = DIRECTION ( 'NONE',  ( 0.000000000000000000, -1.000000000000000000, 0.000000000000000000 ) ) ;
#27443 = CARTESIAN_POINT ( 'NONE',  ( 0.4921259842519685179, -0.03220957031753991784, -1.569881889763779625 ) ) ;
#27444 = SURFACE_SIDE_STYLE ('',( #21883 ) ) ;
#27445 = CIRCLE ( 'NONE', #15287, 0.1298643763538141760 ) ;
#27446 = ORIENTED_EDGE ( 'NONE', *, *, #9584, .F. ) ;
#27447 = ORIENTED_EDGE ( 'NONE', *, *, #11760, .T. ) ;
#27448 = AXIS2_PLACEMENT_3D ( 'NONE', #12793, #6032, #3604 ) ;
#27449 = DIRECTION ( 'NONE',  ( 1.000000000000000000, 0.000000000000000000, 0.000000000000000000 ) ) ;
#27450 = DIRECTION ( 'NONE',  ( 1.000000000000000000, 0.000000000000000000, 0.000000000000000000 ) ) ;
#27451 = PRESENTATION_LAYER_ASSIGNMENT (  '', '', ( #18409 ) ) ;
#27452 = CARTESIAN_POINT ( 'NONE',  ( 0.000000000000000000, 0.000000000000000000, 0.07637795275590551769 ) ) ;
#27453 = DIRECTION ( 'NONE',  ( 0.000000000000000000, 1.000000000000000000, 0.000000000000000000 ) ) ;
#27454 = VERTEX_POINT ( 'NONE', #2997 ) ;
#27455 = CARTESIAN_POINT ( 'NONE',  ( -0.5656587879800142327, -0.5969381639805851902, 0.9446416071465162378 ) ) ;
#27456 = ORIENTED_EDGE ( 'NONE', *, *, #4830, .T. ) ;
#27457 = CARTESIAN_POINT ( 'NONE',  ( -0.6054097002486862333, -0.5184600247616719670, -0.9894322414030318757 ) ) ;
#27458 = VECTOR ( 'NONE', #1701, 39.37007874015748143 ) ;
#27459 = CARTESIAN_POINT ( 'NONE',  ( 0.3019498226894188897, 0.3592501948415138258, 0.07637630773773071424 ) ) ;
#27460 = CARTESIAN_POINT ( 'NONE',  ( -9.069736220472440932E-16, -0.8267716535433070613, 0.7883858267716535861 ) ) ;
#27461 = CARTESIAN_POINT ( 'NONE',  ( 0.4898768902087983768, -2.140741338582677483E-16, 0.2362204724409449064 ) ) ;
#27462 = ADVANCED_FACE ( 'NONE', ( #9932 ), #20613, .F. ) ;
#27463 = VERTEX_POINT ( 'NONE', #27183 ) ;
#27464 = ( CONVERSION_BASED_UNIT ( 'INCH', #5859 ) LENGTH_UNIT ( ) NAMED_UNIT ( #10311 ) ) ;
#27465 = EDGE_CURVE ( 'NONE', #12080, #12707, #7827, .T. ) ;
#27466 = CARTESIAN_POINT ( 'NONE',  ( -0.6102362204724409711, 0.000000000000000000, 0.000000000000000000 ) ) ;
#27467 = ORIENTED_EDGE ( 'NONE', *, *, #20014, .T. ) ;
#27468 = CARTESIAN_POINT ( 'NONE',  ( -0.1584824234590963832, -0.3213085410494903593, -3.115157480314960647 ) ) ;
#27469 = DIRECTION ( 'NONE',  ( 0.000000000000000000, 0.000000000000000000, -1.000000000000000000 ) ) ;
#27470 = EDGE_CURVE ( 'NONE', #11701, #20882, #19124, .T. ) ;
#27471 = AXIS2_PLACEMENT_3D ( 'NONE', #10854, #19469, #8734 ) ;
#27472 = VERTEX_POINT ( 'NONE', #7689 ) ;
#27473 = CARTESIAN_POINT ( 'NONE',  ( -0.02963280468032184270, -0.4527559054764770385, -1.934055118110236338 ) ) ;
#27474 = CIRCLE ( 'NONE', #25202, 0.1181102362204720091 ) ;
#27475 = ADVANCED_FACE ( 'NONE', ( #913 ), #11630, .F. ) ;
#27476 = VECTOR ( 'NONE', #7800, 39.37007874015748143 ) ;
#27477 = CARTESIAN_POINT ( 'NONE',  ( -0.4527559054764770385, 0.000000000000000000, -1.934055118110236338 ) ) ;
#27478 = EDGE_LOOP ( 'NONE', ( #15055, #9050, #12254, #4246, #12400, #5461 ) ) ;
#27479 = CIRCLE ( 'NONE', #14863, 0.003937007874015747977 ) ;
#27480 = CARTESIAN_POINT ( 'NONE',  ( -0.5439522672647024715, -0.3016216585743382028, -0.1264851098546873887 ) ) ;
#27481 = CARTESIAN_POINT ( 'NONE',  ( -0.4777261797697566759, 0.2355331214654138305, 1.747047244094488194 ) ) ;
#27482 = CARTESIAN_POINT ( 'NONE',  ( 0.3988311005573134116, 0.4763376377694984454, 0.09685039370078740717 ) ) ;
#27483 = ADVANCED_FACE ( 'NONE', ( #26888 ), #16166, .T. ) ;
#27484 = VERTEX_POINT ( 'NONE', #9500 ) ;
#27485 = DIRECTION ( 'NONE',  ( 0.000000000000000000, 1.000000000000000000, 0.000000000000000000 ) ) ;
#27486 = CARTESIAN_POINT ( 'NONE',  ( -0.1570784101597038906, -0.3184623230427779395, 1.953740157480314821 ) ) ;
#27487 = CARTESIAN_POINT ( 'NONE',  ( 0.3986320731132086959, -0.2308081338369904478, 0.1771653543307089018 ) ) ;
#27488 = CARTESIAN_POINT ( 'NONE',  ( 0.2173565190940987546, -0.5952284643178856749, 0.2481708550929211665 ) ) ;
#27489 = VERTEX_POINT ( 'NONE', #11775 ) ;
#27490 = CARTESIAN_POINT ( 'NONE',  ( -0.3543307086614173596, -0.02319089060378156514, 1.953740157480315043 ) ) ;
#27491 = ORIENTED_EDGE ( 'NONE', *, *, #26541, .F. ) ;
#27492 = EDGE_LOOP ( 'NONE', ( #23061, #13720, #10704, #15778 ) ) ;
#27493 = ORIENTED_EDGE ( 'NONE', *, *, #15791, .F. ) ;
#27494 = CARTESIAN_POINT ( 'NONE',  ( 0.03532354024591839031, -0.6299212598425196763, 0.000000000000000000 ) ) ;
#27495 = TOROIDAL_SURFACE ( 'NONE', #12132, 0.4232283464566928832, 0.07677165354330708902 ) ;
#27496 = CARTESIAN_POINT ( 'NONE',  ( 0.000000000000000000, 0.000000000000000000, -4.015748031496062964 ) ) ;
#27497 = DIRECTION ( 'NONE',  ( -1.000000000000000000, 0.000000000000000000, 0.000000000000000000 ) ) ;
#27499 = CARTESIAN_POINT ( 'NONE',  ( -0.4954197419817796266, -0.2442565704126152260, 0.9399606299212598381 ) ) ;
#27498 = CARTESIAN_POINT ( 'NONE',  ( 0.2720459371704843088, 0.3242117229735830830, 0.1377952755905511861 ) ) ;
#27500 = AXIS2_PLACEMENT_3D ( 'NONE', #11755, #26722, #22776 ) ;
#27501 = ORIENTED_EDGE ( 'NONE', *, *, #15964, .F. ) ;
#27502 = FACE_OUTER_BOUND ( 'NONE', #14276, .T. ) ;
#27503 = VERTEX_POINT ( 'NONE', #16435 ) ;
#27504 = DIRECTION ( 'NONE',  ( 0.000000000000000000, -1.000000000000000000, 0.000000000000000000 ) ) ;
#27505 = CARTESIAN_POINT ( 'NONE',  ( 0.2647715730835492609, -0.5498038367121063086, 0.2362204724409449064 ) ) ;
#27506 = EDGE_CURVE ( 'NONE', #12497, #26290, #4366, .T. ) ;
#27507 = CARTESIAN_POINT ( 'NONE',  ( -0.2842490391651705806, 0.2180698645301660521, -3.115157480314960647 ) ) ;
#27508 = CARTESIAN_POINT ( 'NONE',  ( 0.1279527559055118058, 0.7552056691248124620, 0.000000000000000000 ) ) ;
#27509 = AXIS2_PLACEMENT_3D ( 'NONE', #12334, #16869, #23229 ) ;
#27510 = CARTESIAN_POINT ( 'NONE',  ( 0.000000000000000000, 0.07874015748031508444, 0.000000000000000000 ) ) ;
#27511 = DIRECTION ( 'NONE',  ( -1.000000000000000000, 0.000000000000000000, 0.000000000000000000 ) ) ;
#27512 = EDGE_CURVE ( 'NONE', #8934, #12846, #9011, .T. ) ;
#27513 = CARTESIAN_POINT ( 'NONE',  ( -0.6299212598425196763, 0.000000000000000000, -0.006889763779527558960 ) ) ;
#27514 = CARTESIAN_POINT ( 'NONE',  ( 0.0006812437162516955368, 0.6577569867585544294, 0.2081850588313099992 ) ) ;
#27515 = EDGE_CURVE ( 'NONE', #12714, #26100, #13897, .T. ) ;
#27516 = ORIENTED_EDGE ( 'NONE', *, *, #14872, .T. ) ;
#27517 = CARTESIAN_POINT ( 'NONE',  ( 0.5708675606921426171, 0.03746919241596965988, 0.9399606299212597271 ) ) ;
#27518 = FACE_OUTER_BOUND ( 'NONE', #25835, .T. ) ;
#27519 = CARTESIAN_POINT ( 'NONE',  ( 0.000000000000000000, 0.000000000000000000, 0.1771653543307086520 ) ) ;
#27520 = AXIS2_PLACEMENT_3D ( 'NONE', #26203, #10959, #17974 ) ;
#27521 = EDGE_CURVE ( 'NONE', #23101, #833, #4663, .T. ) ;
#27522 = CARTESIAN_POINT ( 'NONE',  ( 0.3412792617076849666, 0.05967164814832576214, 0.1276989850568736595 ) ) ;
#27523 = CARTESIAN_POINT ( 'NONE',  ( -0.1378076643338853602, -0.5144970376935932288, 1.747047244094488194 ) ) ;
#27524 = CARTESIAN_POINT ( 'NONE',  ( -0.2131049448083992270, -0.5835666837866889667, 0.09685039370078740717 ) ) ;
#27525 = CARTESIAN_POINT ( 'NONE',  ( -0.03349795313264251895, -0.5118110236220473341, 1.766732283464566899 ) ) ;
#27526 = ORIENTED_EDGE ( 'NONE', *, *, #10164, .F. ) ;
#27527 = DIRECTION ( 'NONE',  ( 0.000000000000000000, 0.000000000000000000, 1.000000000000000000 ) ) ;
#27528 = EDGE_LOOP ( 'NONE', ( #25466, #17660, #22534, #12046 ) ) ;
#27529 = CARTESIAN_POINT ( 'NONE',  ( -0.2309201403895324856, -0.4006498629591504490, -1.928289503579156516 ) ) ;
#27530 = CARTESIAN_POINT ( 'NONE',  ( 0.3771653543307086909, 0.000000000000000000, 0.07637795275590551769 ) ) ;
#27531 = CARTESIAN_POINT ( 'NONE',  ( 0.3007905576423847704, 0.1482986320106501610, 1.973425196850393970 ) ) ;
#27532 = ORIENTED_EDGE ( 'NONE', *, *, #24777, .F. ) ;
#27533 = ORIENTED_EDGE ( 'NONE', *, *, #17896, .F. ) ;
#27534 = CARTESIAN_POINT ( 'NONE',  ( 0.1294857240059045234, -0.3542416573274181357, 0.1992125984251968684 ) ) ;
#27535 = CARTESIAN_POINT ( 'NONE',  ( 0.000000000000000000, 0.000000000000000000, -4.330708661417323135 ) ) ;
#27536 = ORIENTED_EDGE ( 'NONE', *, *, #23846, .F. ) ;
#27537 = ORIENTED_EDGE ( 'NONE', *, *, #12030, .F. ) ;
#27538 = AXIS2_PLACEMENT_3D ( 'NONE', #2128, #12715, #12993 ) ;
#27539 = EDGE_CURVE ( 'NONE', #2920, #6078, #3915, .T. ) ;
#27540 = B_SPLINE_CURVE_WITH_KNOTS ( 'NONE', 3,
 ( #23886, #17377, #13129, #8480, #12712, #6235, #17100, #19490, #25855, #185 ),
 .UNSPECIFIED., .F., .F.,
 ( 4, 2, 2, 2, 4 ),
 ( 0.000000000000000000, 0.2500000000000000000, 0.5000000000000000000, 0.7500000000000000000, 1.000000000000000000 ),
 .UNSPECIFIED. ) ;
#27541 = AXIS2_PLACEMENT_3D ( 'NONE', #3942, #5931, #8327 ) ;
#27542 = CONTEXT_DEPENDENT_SHAPE_REPRESENTATION ( #9410, #20668 ) ;
#27543 = CARTESIAN_POINT ( 'NONE',  ( 2.483043706889356121E-16, 0.07874015748031495954, -1.988188976307287970 ) ) ;
#27544 = CARTESIAN_POINT ( 'NONE',  ( 0.4621283342336243716, 0.08168108835551360358, 0.1992150590373740204 ) ) ;
#27545 = CARTESIAN_POINT ( 'NONE',  ( -0.03532354024591771724, -0.6299212598425196763, -0.6299212598425196763 ) ) ;
#27546 = EDGE_CURVE ( 'NONE', #19464, #21657, #14080, .T. ) ;
#27547 = TOROIDAL_SURFACE ( 'NONE', #15379, 0.4232283464566928832, 0.07677165354330708902 ) ;
#27548 = ORIENTED_EDGE ( 'NONE', *, *, #14157, .F. ) ;
#27549 = CARTESIAN_POINT ( 'NONE',  ( 0.4157391792961063204, 0.3323952789219082882, 0.3401574803149606252 ) ) ;
#27550 = ADVANCED_BREP_SHAPE_REPRESENTATION ( 'Rear Bearing Cover', ( #11975, #11588 ), #19278 ) ;
#27551 = CARTESIAN_POINT ( 'NONE',  ( -6.750021727583836750E-17, -0.5511811023622047445, 0.01181102362204724393 ) ) ;
#27552 = DIRECTION ( 'NONE',  ( 0.000000000000000000, 0.000000000000000000, -1.000000000000000000 ) ) ;
#27553 = DIRECTION ( 'NONE',  ( 0.000000000000000000, 0.000000000000000000, 1.000000000000000000 ) ) ;
#27554 = CARTESIAN_POINT ( 'NONE',  ( -0.5988895145664465680, -0.2041512096132067910, 0.2199573444130424604 ) ) ;
#27555 = CARTESIAN_POINT ( 'NONE',  ( -0.4621283342336283129, 0.08168108835549449387, 0.07637549214372854611 ) ) ;
#27556 = CARTESIAN_POINT ( 'NONE',  ( -0.1771653543307086520, 0.000000000000000000, 0.000000000000000000 ) ) ;
#27557 = DIRECTION ( 'NONE',  ( 0.000000000000000000, 0.000000000000000000, 1.000000000000000000 ) ) ;
#27558 = FACE_OUTER_BOUND ( 'NONE', #13975, .T. ) ;
#27559 = AXIS2_PLACEMENT_3D ( 'NONE', #27505, #14233, #24942 ) ;
#27560 = DIRECTION ( 'NONE',  ( 0.000000000000000000, 0.000000000000000000, 1.000000000000000000 ) ) ;
#27561 = ORIENTED_EDGE ( 'NONE', *, *, #26820, .T. ) ;
#27562 = CARTESIAN_POINT ( 'NONE',  ( -0.06889763779527552368, 0.000000000000000000, -0.3779527559055118058 ) ) ;
#27563 = ORIENTED_EDGE ( 'NONE', *, *, #3654, .T. ) ;
#27564 = AXIS2_PLACEMENT_3D ( 'NONE', #3458, #18284, #26930 ) ;
#27565 = CARTESIAN_POINT ( 'NONE',  ( 0.4930758245789425009, 0.08754571829529310401, 0.09685039370078740717 ) ) ;
#27566 = DIRECTION ( 'NONE',  ( 0.000000000000000000, 0.000000000000000000, -1.000000000000000000 ) ) ;
#27567 = CARTESIAN_POINT ( 'NONE',  ( -0.4954197419817560344, 0.2442565704126489212, 0.9202755905511811330 ) ) ;
#27568 = ORIENTED_EDGE ( 'NONE', *, *, #4796, .F. ) ;
#27569 = CARTESIAN_POINT ( 'NONE',  ( -0.5177165354330708347, -0.4724409448818898127, -0.6411263657805729155 ) ) ;
#27570 = ORIENTED_EDGE ( 'NONE', *, *, #14446, .F. ) ;
#27571 = ( NAMED_UNIT ( * ) PLANE_ANGLE_UNIT ( ) SI_UNIT ( $, .RADIAN. ) ) ;
#27572 = CARTESIAN_POINT ( 'NONE',  ( -0.8031496062992127261, 9.980389268641816488E-17, -1.092739370078740131E-17 ) ) ;
#27573 = LINE ( 'NONE', #10041, #9531 ) ;
#27574 = EDGE_CURVE ( 'NONE', #10266, #9518, #10212, .T. ) ;
#27575 = B_SPLINE_CURVE_WITH_KNOTS ( 'NONE', 3,
 ( #11489, #13336, #21961, #21820, #8949, #21687 ),
 .UNSPECIFIED., .F., .F.,
 ( 4, 2, 4 ),
 ( 1.162880698919837918, 1.164573402063411978, 1.166266105206986037 ),
 .UNSPECIFIED. ) ;
#27576 = AXIS2_PLACEMENT_3D ( 'NONE', #23416, #25515, #13072 ) ;
#27577 = CYLINDRICAL_SURFACE ( 'NONE', #13212, 0.09842519685039370636 ) ;
#27578 = EDGE_LOOP ( 'NONE', ( #20743, #25241, #23594, #17646 ) ) ;
#27579 = CARTESIAN_POINT ( 'NONE',  ( -0.6514872030408946912, 0.1141809932447457321, 0.1616495878811869680 ) ) ;
#27580 = CARTESIAN_POINT ( 'NONE',  ( 0.5376957092749897749, -0.3112026930391976753, 0.2574803149606298969 ) ) ;
#27581 = ORIENTED_EDGE ( 'NONE', *, *, #22970, .F. ) ;
#27582 = CARTESIAN_POINT ( 'NONE',  ( 0.04380447413659065842, -0.3324885138898235892, 1.973425196850393970 ) ) ;
#27583 = LINE ( 'NONE', #10609, #25224 ) ;
#27584 = CARTESIAN_POINT ( 'NONE',  ( 0.1755067523729419432, -0.3028750839302637998, -0.5245950337139047015 ) ) ;
#27585 = TOROIDAL_SURFACE ( 'NONE', #24392, 0.6102362204724409711, 0.1299212598425196763 ) ;
#27586 = CARTESIAN_POINT ( 'NONE',  ( 0.1775991818008549328, -0.5230301363771188150, 0.9399606299212598381 ) ) ;
#27587 = CARTESIAN_POINT ( 'NONE',  ( 0.1599629598573824862, -0.4411872753631803090, 0.07637795275590551769 ) ) ;
#27588 = ORIENTED_EDGE ( 'NONE', *, *, #16301, .F. ) ;
#27589 = CARTESIAN_POINT ( 'NONE',  ( 0.000000000000000000, 0.9055118110236217710, 0.000000000000000000 ) ) ;
#27590 = CARTESIAN_POINT ( 'NONE',  ( 0.2662775206740974898, 0.4613022222209450796, 1.747047244094488194 ) ) ;
#27591 = EDGE_LOOP ( 'NONE', ( #20008, #25633, #2934, #14789 ) ) ;
#27592 = EDGE_CURVE ( 'NONE', #3555, #17381, #27850, .T. ) ;
#27593 = AXIS2_PLACEMENT_3D ( 'NONE', #18822, #12062, #7969 ) ;
#27594 = CARTESIAN_POINT ( 'NONE',  ( -0.4889536969034878333, -0.06441834428466509943, -1.550196850393700920 ) ) ;
#27595 = ORIENTED_EDGE ( 'NONE', *, *, #11626, .T. ) ;
#27596 = DIRECTION ( 'NONE',  ( 0.000000000000000000, 0.000000000000000000, 1.000000000000000000 ) ) ;
#27597 = CARTESIAN_POINT ( 'NONE',  ( -0.7874015748031496509, 0.000000000000000000, -1.052618110236220428 ) ) ;
#27598 = FACE_OUTER_BOUND ( 'NONE', #8048, .T. ) ;
#27599 = CARTESIAN_POINT ( 'NONE',  ( 0.5314960629921260393, 0.000000000000000000, 1.747047244094488194 ) ) ;
#27600 = ORIENTED_EDGE ( 'NONE', *, *, #23833, .T. ) ;
#27601 = LINE ( 'NONE', #8244, #3379 ) ;
#27602 = VERTEX_POINT ( 'NONE', #6658 ) ;
#27603 = AXIS2_PLACEMENT_3D ( 'NONE', #9433, #9290, #18033 ) ;
#27604 = DIRECTION ( 'NONE',  ( -1.000000000000000000, 0.000000000000000000, 0.000000000000000000 ) ) ;
#27605 = EDGE_CURVE ( 'NONE', #2522, #1348, #2106, .T. ) ;
#27606 = CARTESIAN_POINT ( 'NONE',  ( -0.3661417322834645272, 0.9448818897637796255, -1.639108661417322569E-17 ) ) ;
#27607 = DIRECTION ( 'NONE',  ( 1.000000000000000000, 0.000000000000000000, 0.000000000000000000 ) ) ;
#27608 = CARTESIAN_POINT ( 'NONE',  ( 0.1632039128452630883, -0.4501088385450159879, 0.1920935997052418687 ) ) ;
#27609 = EDGE_LOOP ( 'NONE', ( #629, #15705, #7725, #22333 ) ) ;
#27610 = CARTESIAN_POINT ( 'NONE',  ( -4.618943439303797186E-17, -0.3771653543307086909, 0.03818897637795275884 ) ) ;
#27611 = FACE_OUTER_BOUND ( 'NONE', #24537, .T. ) ;
#27612 = DIRECTION ( 'NONE',  ( -0.9659258263664933786, -0.2588190448135661570, 0.000000000000000000 ) ) ;
#27613 = CARTESIAN_POINT ( 'NONE',  ( -0.07874015748031495954, -0.04546065111729338803, -0.3779527559055118058 ) ) ;
#27614 = CARTESIAN_POINT ( 'NONE',  ( -0.4438564651657478377, 0.1188866373884873845, -1.928289503579152742 ) ) ;
#27615 = CIRCLE ( 'NONE', #22188, 1.092519685039370136 ) ;
#27616 = CARTESIAN_POINT ( 'NONE',  ( -0.2490711204941346568, 1.208528701367826752, -0.6047752023237676910 ) ) ;
#27617 = STYLED_ITEM ( 'NONE', ( #12911 ), #12666 ) ;
#27618 = EDGE_CURVE ( 'NONE', #657, #26100, #9293, .T. ) ;
#27619 = ORIENTED_EDGE ( 'NONE', *, *, #4066, .T. ) ;
#27620 = VERTEX_POINT ( 'NONE', #8762 ) ;
#27621 = ORIENTED_EDGE ( 'NONE', *, *, #18511, .F. ) ;
#27622 = CARTESIAN_POINT ( 'NONE',  ( -0.6002615430280354714, -0.1506498012739275749, -0.09040378142097618697 ) ) ;
#27623 = CARTESIAN_POINT ( 'NONE',  ( 0.000000000000000000, 0.000000000000000000, -0.05511811023622047168 ) ) ;
#27624 = EDGE_LOOP ( 'NONE', ( #25989, #14994, #15903, #8043 ) ) ;
#27625 = ORIENTED_EDGE ( 'NONE', *, *, #232, .T. ) ;
#27626 = DIRECTION ( 'NONE',  ( -1.000000000000000000, 0.000000000000000000, 0.000000000000000000 ) ) ;
#27627 = DIRECTION ( 'NONE',  ( 0.000000000000000000, 0.000000000000000000, 1.000000000000000000 ) ) ;
#27628 = PRODUCT ( 'Cam Follower', 'Cam Follower', '', ( #22388 ) ) ;
#27629 = CARTESIAN_POINT ( 'NONE',  ( 0.2256062985769322349, -0.6178563876516726117, 0.1461456498233222601 ) ) ;
#27630 = ADVANCED_FACE ( 'NONE', ( #10070 ), #7977, .F. ) ;
#27631 = VERTEX_POINT ( 'NONE', #25999 ) ;
#27632 = TOROIDAL_SURFACE ( 'NONE', #25429, 0.3070866141732283561, 0.01181102362204724393 ) ;
#27633 = CARTESIAN_POINT ( 'NONE',  ( -0.3184841198566451537, -0.1570220809524492667, 1.953740157480315043 ) ) ;
#27634 = EDGE_LOOP ( 'NONE', ( #4704, #3017, #9178, #1346 ) ) ;
#27635 = CIRCLE ( 'NONE', #17267, 0.6212598425196850238 ) ;
#27636 = CARTESIAN_POINT ( 'NONE',  ( -0.5439122934449801550, -0.2529464855333863893, -0.2763027211839643171 ) ) ;
#27637 = DIRECTION ( 'NONE',  ( 1.000000000000000000, 0.000000000000000000, 0.000000000000000000 ) ) ;
#27639 = CARTESIAN_POINT ( 'NONE',  ( 0.1480156394741928561, -0.5526079293736928522, 0.9399606299212598381 ) ) ;
#27638 = FACE_OUTER_BOUND ( 'NONE', #4786, .T. ) ;
#27640 = EDGE_CURVE ( 'NONE', #8867, #20727, #11566, .T. ) ;
#27641 = DIRECTION ( 'NONE',  ( -0.000000000000000000, -1.000000000000000000, -0.000000000000000000 ) ) ;
#27642 = ORIENTED_EDGE ( 'NONE', *, *, #3593, .T. ) ;
#27643 = EDGE_LOOP ( 'NONE', ( #4034, #24489, #7294, #1887 ) ) ;
#27644 = CARTESIAN_POINT ( 'NONE',  ( -0.7165354330708662012, 8.775028245858987528E-17, 0.01181102362204724393 ) ) ;
#27645 = FACE_OUTER_BOUND ( 'NONE', #24137, .T. ) ;
#27646 = AXIS2_PLACEMENT_3D ( 'NONE', #27651, #8295, #16912 ) ;
#27647 = CARTESIAN_POINT ( 'NONE',  ( -0.2180698645301862859, 0.2842490391651604775, -3.115157480314960647 ) ) ;
#27648 = DIRECTION ( 'NONE',  ( 1.000000000000000000, 0.000000000000000000, 0.000000000000000000 ) ) ;
#27649 = CARTESIAN_POINT ( 'NONE',  ( 0.3169330146499940715, -0.1835719822052965799, 0.1910323753043391970 ) ) ;
#27650 = CARTESIAN_POINT ( 'NONE',  ( 0.6239291699165746552, 0.1106940470469692378, 0.1061598535670113391 ) ) ;
#27651 = CARTESIAN_POINT ( 'NONE',  ( 0.000000000000000000, 0.000000000000000000, 0.1377952755905511861 ) ) ;
#27652 = CARTESIAN_POINT ( 'NONE',  ( 0.0006681923949035713933, 0.6336721034125017971, 0.1061598535669395216 ) ) ;
#27653 = VECTOR ( 'NONE', #22788, 39.37007874015748143 ) ;
#27654 = ORIENTED_EDGE ( 'NONE', *, *, #24462, .T. ) ;
#27655 = CARTESIAN_POINT ( 'NONE',  ( -0.5417516942597173646, 0.1838445375788849978, 0.9399606299212601712 ) ) ;
#27656 = VERTEX_POINT ( 'NONE', #20811 ) ;
#27657 = ORIENTED_EDGE ( 'NONE', *, *, #23992, .F. ) ;
#27658 = CARTESIAN_POINT ( 'NONE',  ( -0.6116756676109479374, 0.4474965194255770551, -0.3672460818887063327 ) ) ;
#27659 = FILL_AREA_STYLE ('',( #14392 ) ) ;
#27660 = CARTESIAN_POINT ( 'NONE',  ( -0.2395669291338582696, 0.000000000000000000, -0.02362204724409448786 ) ) ;
#27661 = ORIENTED_EDGE ( 'NONE', *, *, #24629, .F. ) ;
#27662 = EDGE_CURVE ( 'NONE', #5267, #26096, #26020, .T. ) ;
#27663 = AXIS2_PLACEMENT_3D ( 'NONE', #26343, #507, #15493 ) ;
#27664 = ORIENTED_EDGE ( 'NONE', *, *, #5950, .F. ) ;
#27665 = CARTESIAN_POINT ( 'NONE',  ( 0.2180698645301765992, 0.2842490391651533721, -3.115157480314960647 ) ) ;
#27666 = CARTESIAN_POINT ( 'NONE',  ( 0.000000000000000000, 0.000000000000000000, 1.953740157480315043 ) ) ;
#27667 = CARTESIAN_POINT ( 'NONE',  ( 0.0006615832606325197825, 0.6212594902576319411, 0.09685039370078740717 ) ) ;
#27668 = EDGE_CURVE ( 'NONE', #6614, #25145, #15221, .T. ) ;
#27669 = CARTESIAN_POINT ( 'NONE',  ( 0.2521176338356617697, -0.2211428102655709493, 1.973425196850393970 ) ) ;
#27670 = ORIENTED_EDGE ( 'NONE', *, *, #1078, .F. ) ;
#27671 = EDGE_LOOP ( 'NONE', ( #13623, #3315, #6864, #10990 ) ) ;
#27672 = CARTESIAN_POINT ( 'NONE',  ( 0.000000000000000000, 0.5905511811023621549, 0.000000000000000000 ) ) ;
#27673 = VERTEX_POINT ( 'NONE', #15002 ) ;
#27674 = ORIENTED_EDGE ( 'NONE', *, *, #10642, .F. ) ;
#27675 = AXIS2_PLACEMENT_3D ( 'NONE', #4079, #3937, #10560 ) ;
#27676 = AXIS2_PLACEMENT_3D ( 'NONE', #27718, #8219, #16839 ) ;
#27677 = DIRECTION ( 'NONE',  ( 1.000000000000000000, 0.000000000000000000, 0.000000000000000000 ) ) ;
#27678 = CARTESIAN_POINT ( 'NONE',  ( -0.2427018018350767803, 0.2887032559529634224, 0.1992142436757342316 ) ) ;
#27679 = DIRECTION ( 'NONE',  ( 0.000000000000000000, 0.000000000000000000, -1.000000000000000000 ) ) ;
#27680 = EDGE_LOOP ( 'NONE', ( #2787, #22441 ) ) ;
#27681 = CIRCLE ( 'NONE', #19979, 1.092519685039370136 ) ;
#27682 = B_SPLINE_CURVE_WITH_KNOTS ( 'NONE', 3,
 ( #12481, #2669, #21101, #5998, #6146, #14634, #14777, #24016 ),
 .UNSPECIFIED., .F., .F.,
 ( 4, 2, 2, 4 ),
 ( 0.000000000000000000, 0.1250000000000001943, 0.2500000000000003886, 0.5000000000000000000 ),
 .UNSPECIFIED. ) ;
#27683 = VERTEX_POINT ( 'NONE', #23620 ) ;
#27684 = ( REPRESENTATION_RELATIONSHIP ('NONE','NONE', #12434, #6338 ) REPRESENTATION_RELATIONSHIP_WITH_TRANSFORMATION ( #1127 )SHAPE_REPRESENTATION_RELATIONSHIP( ) ) ;
#27685 = AXIS2_PLACEMENT_3D ( 'NONE', #5364, #3220, #20476 ) ;
#27686 = DIRECTION ( 'NONE',  ( 0.000000000000000000, 7.180547321999995381E-06, -0.9999999999742197332 ) ) ;
#27687 = DIRECTION ( 'NONE',  ( 0.000000000000000000, 0.000000000000000000, 1.000000000000000000 ) ) ;
#27688 = CARTESIAN_POINT ( 'NONE',  ( -0.4331766658145966287, -0.8171300860253869480, -0.05592082628871295619 ) ) ;
#27689 = CARTESIAN_POINT ( 'NONE',  ( 0.3024344094364739277, 0.3935368318888683437, -1.569881889763779625 ) ) ;
#27690 = AXIS2_PLACEMENT_3D ( 'NONE', #2841, #2334, #11612 ) ;
#27691 = AXIS2_PLACEMENT_3D ( 'NONE', #25078, #26925, #3169 ) ;
#27692 = CARTESIAN_POINT ( 'NONE',  ( 0.08600259748439817442, 0.1968503937007873850, -3.223068998490986825 ) ) ;
#27693 = CARTESIAN_POINT ( 'NONE',  ( -0.09842519685039370636, 0.5905905511811023745, -3.272637795275590733 ) ) ;
#27695 = EDGE_CURVE ( 'NONE', #1869, #6477, #11028, .T. ) ;
#27694 = ORIENTED_EDGE ( 'NONE', *, *, #14827, .F. ) ;
#27696 = CARTESIAN_POINT ( 'NONE',  ( 0.000000000000000000, 0.000000000000000000, -0.07578740157480315376 ) ) ;
#27697 = CARTESIAN_POINT ( 'NONE',  ( 0.5187889641967551313, -0.1190953285357214675, 0.3401574803149606252 ) ) ;
#27698 = LINE ( 'NONE', #14433, #16387 ) ;
#27699 = EDGE_CURVE ( 'NONE', #16461, #12825, #26461, .T. ) ;
#27700 = ORIENTED_EDGE ( 'NONE', *, *, #6203, .T. ) ;
#27701 = CIRCLE ( 'NONE', #1977, 0.5007874015748031704 ) ;
#27702 = VERTEX_POINT ( 'NONE', #21626 ) ;
#27703 = CARTESIAN_POINT ( 'NONE',  ( -0.3382184156749069581, -0.3855916753034488997, -1.550196850393700920 ) ) ;
#27704 = DIRECTION ( 'NONE',  ( 0.000000000000000000, 1.000000000000000000, 0.000000000000000000 ) ) ;
#27705 = FACE_OUTER_BOUND ( 'NONE', #10557, .T. ) ;
#27706 = AXIS2_PLACEMENT_3D ( 'NONE', #14278, #21038, #12280 ) ;
#27707 = CARTESIAN_POINT ( 'NONE',  ( 0.3031496062992122820, 3.784833611538078052E-17, -0.02362204724409448786 ) ) ;
#27708 = ORIENTED_EDGE ( 'NONE', *, *, #55, .T. ) ;
#27709 = ADVANCED_FACE ( 'NONE', ( #10882 ), #19497, .F. ) ;
#27710 = B_SPLINE_CURVE_WITH_KNOTS ( 'NONE', 3,
 ( #16908, #6314, #12522, #21140 ),
 .UNSPECIFIED., .F., .F.,
 ( 4, 4 ),
 ( 0.9031406754215589583, 0.9046454396443728285 ),
 .UNSPECIFIED. ) ;
#27711 = DIRECTION ( 'NONE',  ( -1.000000000000000000, 0.000000000000000000, 0.000000000000000000 ) ) ;
#27712 = ORIENTED_EDGE ( 'NONE', *, *, #6812, .F. ) ;
#27713 = PLANE ( 'NONE',  #27152 ) ;
#27714 = CARTESIAN_POINT ( 'NONE',  ( 0.4792483803807430776, 0.08390985360578698260, 0.2467937633143996445 ) ) ;
#27715 = DIRECTION ( 'NONE',  ( 0.000000000000000000, 0.000000000000000000, 1.000000000000000000 ) ) ;
#27716 = AXIS2_PLACEMENT_3D ( 'NONE', #8228, #14461, #16850 ) ;
#27717 = ADVANCED_FACE ( 'NONE', ( #9747, #14544 ), #19026, .T. ) ;
#27718 = CARTESIAN_POINT ( 'NONE',  ( -2.685748425196850164E-17, 0.000000000000000000, -1.934055118110236338 ) ) ;
#27719 = ORIENTED_EDGE ( 'NONE', *, *, #25354, .T. ) ;
#27720 = DIRECTION ( 'NONE',  ( 0.000000000000000000, 0.000000000000000000, 1.000000000000000000 ) ) ;
#27721 = DIRECTION ( 'NONE',  ( 0.000000000000000000, -1.000000000000000000, 0.000000000000000000 ) ) ;
#27722 = VERTEX_POINT ( 'NONE', #27660 ) ;
#27723 = EDGE_LOOP ( 'NONE', ( #8235, #23616 ) ) ;
#27724 = CARTESIAN_POINT ( 'NONE',  ( -0.1078280746903979848, 0.3175540113612246862, 1.953740157480315043 ) ) ;
#27725 = CARTESIAN_POINT ( 'NONE',  ( -0.01968503937007897581, 0.000000000000000000, 0.000000000000000000 ) ) ;
#27726 = CIRCLE ( 'NONE', #2855, 0.01181102362204724046 ) ;
#27727 = CARTESIAN_POINT ( 'NONE',  ( -0.5671862884095143498, 0.07472527936311554320, 0.9399606299212598381 ) ) ;
#27728 = DIRECTION ( 'NONE',  ( 1.000000000000000000, 0.000000000000000000, 0.000000000000000000 ) ) ;
#27729 = AXIS2_PLACEMENT_3D ( 'NONE', #12050, #27311, #21236 ) ;
#27730 = PLANE ( 'NONE',  #6064 ) ;
#27731 = ORIENTED_EDGE ( 'NONE', *, *, #11322, .T. ) ;
#27732 = CARTESIAN_POINT ( 'NONE',  ( 0.1791085948259714400, 0.3102804211135531398, -3.115157480314960647 ) ) ;
#27733 = DIRECTION ( 'NONE',  ( 1.000000000000000000, 0.000000000000000000, 0.000000000000000000 ) ) ;
#27734 = EDGE_CURVE ( 'NONE', #22409, #10034, #14824, .T. ) ;
#27735 = CIRCLE ( 'NONE', #24536, 0.4842519685039370358 ) ;
#27736 = ORIENTED_EDGE ( 'NONE', *, *, #17454, .T. ) ;
#27737 = EDGE_CURVE ( 'NONE', #7888, #14583, #20204, .T. ) ;
#27738 = CARTESIAN_POINT ( 'NONE',  ( -0.4669911931914537129, -0.1585706980422384171, -1.550196850393700920 ) ) ;
#27739 = CARTESIAN_POINT ( 'NONE',  ( 0.2860009521618275818, -0.4954734376826439579, 0.9399606299212600602 ) ) ;
#27740 = CARTESIAN_POINT ( 'NONE',  ( 0.000000000000000000, 0.000000000000000000, -0.2204724409448818867 ) ) ;
#27741 = CARTESIAN_POINT ( 'NONE',  ( 0.000000000000000000, 0.000000000000000000, -0.2204724409448818867 ) ) ;
#27742 = CARTESIAN_POINT ( 'NONE',  ( 0.2356229156554159598, -0.4776874499715153544, 1.747047244094488194 ) ) ;
#27743 = CARTESIAN_POINT ( 'NONE',  ( -0.0007882571242868541359, 0.7401570605733206465, 0.2161412452779228888 ) ) ;
#27744 = EDGE_LOOP ( 'NONE', ( #4949, #18230, #6308 ) ) ;
#27745 = CARTESIAN_POINT ( 'NONE',  ( -0.2938049579018679469, -0.3349573549949684259, -1.934055118110236338 ) ) ;
#27746 = CARTESIAN_POINT ( 'NONE',  ( -0.6212848329275697523, -0.6280848967520035186, -0.9045786101299029269 ) ) ;
#27747 = CARTESIAN_POINT ( 'NONE',  ( -0.09522017135408125665, 0.3002250880419695678, -3.246903465181130599 ) ) ;
#27748 = AXIS2_PLACEMENT_3D ( 'NONE', #5609, #14083, #22991 ) ;
#27749 = DIRECTION ( 'NONE',  ( 1.000000000000000000, 0.000000000000000000, 0.000000000000000000 ) ) ;
#27750 = CARTESIAN_POINT ( 'NONE',  ( 0.5869493968219645641, -0.4267795243146149664, 5.226543307086613929E-17 ) ) ;
#27751 = CARTESIAN_POINT ( 'NONE',  ( 0.000000000000000000, 0.3937007874015748254, 0.3425196850393700809 ) ) ;
#27752 = ORIENTED_EDGE ( 'NONE', *, *, #18240, .T. ) ;
#27753 = DIRECTION ( 'NONE',  ( 0.000000000000000000, -1.000000000000000000, 0.000000000000000000 ) ) ;
#27754 = ORIENTED_EDGE ( 'NONE', *, *, #23661, .T. ) ;
#27755 = CARTESIAN_POINT ( 'NONE',  ( -0.1275996891957738577, 0.4763861460130593972, -1.550196850393700920 ) ) ;
#27756 = VECTOR ( 'NONE', #26618, 39.37007874015748854 ) ;
#27757 = PRODUCT_DEFINITION_CONTEXT ( 'detailed design', #11784, 'design' ) ;
#27758 = EDGE_CURVE ( 'NONE', #25113, #23041, #9662, .T. ) ;
#27759 = CARTESIAN_POINT ( 'NONE',  ( -0.4296318976989931815, -0.1458850421962362698, -1.934055118110236338 ) ) ;
#27760 = ORIENTED_EDGE ( 'NONE', *, *, #17780, .T. ) ;
#27761 = AXIS2_PLACEMENT_3D ( 'NONE', #3534, #7940, #1430 ) ;
#27762 = CARTESIAN_POINT ( 'NONE',  ( -0.5833277509429386498, -0.2269466161323728526, 0.05590316927886188753 ) ) ;
#27763 = FILL_AREA_STYLE ('',( #25208 ) ) ;
#27764 = CARTESIAN_POINT ( 'NONE',  ( 0.03478633594543814600, -0.5314960629921260393, 1.747047244094488194 ) ) ;
#27765 = CARTESIAN_POINT ( 'NONE',  ( -0.2956505864974143805, 0.3532288989643735944, 0.1639447408836617603 ) ) ;
#27766 = ORIENTED_EDGE ( 'NONE', *, *, #18319, .F. ) ;
#27767 = FACE_BOUND ( 'NONE', #15282, .T. ) ;
#27768 = CARTESIAN_POINT ( 'NONE',  ( -0.6003337592290733937, -0.5548708868587087784, 0.9753553170054337640 ) ) ;
#27769 = CARTESIAN_POINT ( 'NONE',  ( 0.3986320731132085848, -0.2308081338369909197, 0.1903859677802542949 ) ) ;
#27770 = CARTESIAN_POINT ( 'NONE',  ( -0.1361267291514174083, -0.2631590568957330456, 0.2159117096782867951 ) ) ;
#27771 = VECTOR ( 'NONE', #14101, 39.37007874015748854 ) ;
#27772 = ORIENTED_EDGE ( 'NONE', *, *, #23935, .T. ) ;
#27773 = CARTESIAN_POINT ( 'NONE',  ( 0.2817310484609195642, 0.2161381151962948888, 1.953740157480315043 ) ) ;
#27774 = ORIENTED_EDGE ( 'NONE', *, *, #3964, .T. ) ;
#27775 = CARTESIAN_POINT ( 'NONE',  ( -0.5618798588062663413, -0.2119744112645649270, -0.2642172244137618309 ) ) ;
#27776 = CARTESIAN_POINT ( 'NONE',  ( 0.3772436174784425389, -0.4300830224589218265, 0.9399606299212598381 ) ) ;
#27777 = CARTESIAN_POINT ( 'NONE',  ( 0.000000000000000000, 0.000000000000000000, 2.504921259842519898 ) ) ;
#27778 = ORIENTED_EDGE ( 'NONE', *, *, #5174, .T. ) ;
#27779 = SPHERICAL_SURFACE ( 'NONE', #6968, 0.07677362204724409722 ) ;
#27780 = DIRECTION ( 'NONE',  ( 0.000000000000000000, 0.000000000000000000, 1.000000000000000000 ) ) ;
#27781 = VECTOR ( 'NONE', #13160, 39.37007874015748854 ) ;
#27782 = CARTESIAN_POINT ( 'NONE',  ( 0.09660931395005455113, -0.3606853515406215904, -3.115157480314960647 ) ) ;
#27783 = CARTESIAN_POINT ( 'NONE',  ( -0.03532354024591901481, 0.000000000000000000, 0.000000000000000000 ) ) ;
#27784 = CARTESIAN_POINT ( 'NONE',  ( -0.03937007874015747977, 0.6299212598425196763, 0.000000000000000000 ) ) ;
#27785 = PLANE ( 'NONE',  #26573 ) ;
#27786 = EDGE_CURVE ( 'NONE', #17040, #5138, #14796, .T. ) ;
#27787 = SHAPE_REPRESENTATION ( 'O-Ring 26.5x2.65', ( #11588 ), #16570 ) ;
#27788 = CARTESIAN_POINT ( 'NONE',  ( 0.4061284506584276199, -0.2351468520616558922, 0.07637795275590551769 ) ) ;
#27789 = AXIS2_PLACEMENT_3D ( 'NONE', #10100, #6296, #18709 ) ;
#27790 = B_SPLINE_CURVE_WITH_KNOTS ( 'NONE', 3,
 ( #22354, #23565, #4197, #18078, #21431, #6321 ),
 .UNSPECIFIED., .F., .F.,
 ( 4, 2, 4 ),
 ( 0.4045103800602299904, 0.4064350009536160102, 0.4083596218470010308 ),
 .UNSPECIFIED. ) ;
#27791 = CARTESIAN_POINT ( 'NONE',  ( -2.272295064268543552, 0.6488494047548032384, 1.633858267716535639 ) ) ;
#27792 = CARTESIAN_POINT ( 'NONE',  ( -0.4783323773986817851, 0.2762247810518556612, 0.9202755905511811330 ) ) ;
#27793 = EDGE_CURVE ( 'NONE', #16039, #9880, #16549, .T. ) ;
#27794 = VECTOR ( 'NONE', #8679, 39.37007874015748143 ) ;
#27795 = SPHERICAL_SURFACE ( 'NONE', #11539, 0.07677362204724409722 ) ;
#27796 = CARTESIAN_POINT ( 'NONE',  ( -0.2530785775239965951, 0.5130740159366039554, 0.9399606299212602822 ) ) ;
#27797 = ORIENTED_EDGE ( 'NONE', *, *, #12242, .T. ) ;
#27798 = VERTEX_POINT ( 'NONE', #7353 ) ;
#27799 = EDGE_CURVE ( 'NONE', #24778, #3153, #3941, .T. ) ;
#27800 = ADVANCED_FACE ( 'NONE', ( #6196 ), #2955, .T. ) ;
#27801 = VERTEX_POINT ( 'NONE', #13997 ) ;
#27802 = DIRECTION ( 'NONE',  ( 0.000000000000000000, 0.000000000000000000, -1.000000000000000000 ) ) ;
#27803 = CARTESIAN_POINT ( 'NONE',  ( -0.4600326175560542907, 0.2268096725222489285, 1.766732283464566899 ) ) ;
#27804 = VERTEX_POINT ( 'NONE', #11727 ) ;
#27805 = VERTEX_POINT ( 'NONE', #869 ) ;
#27806 = CARTESIAN_POINT ( 'NONE',  ( -0.3726024258163779246, 0.02438677169354841121, -3.115157480314960647 ) ) ;
#27807 = VECTOR ( 'NONE', #2387, 39.37007874015748854 ) ;
#27808 = CARTESIAN_POINT ( 'NONE',  ( 0.5869493968219645641, -0.2133897621573074832, 0.3696019098714952711 ) ) ;
#27809 = DIRECTION ( 'NONE',  ( -0.5000000010362839475, -1.060575237992202059E-16, 0.8660254031861397417 ) ) ;
#27810 = CARTESIAN_POINT ( 'NONE',  ( 0.2041304421298337501, 0.2660793235464286033, 1.973425196850393970 ) ) ;
#27811 = VERTEX_POINT ( 'NONE', #3919 ) ;
#27812 = ORIENTED_EDGE ( 'NONE', *, *, #4650, .T. ) ;
#27813 = CIRCLE ( 'NONE', #8856, 0.4456396174367268093 ) ;
#27814 = CARTESIAN_POINT ( 'NONE',  ( 0.3707612262533033776, -0.3252100150720387273, -1.550196850393700920 ) ) ;
#27815 = EDGE_LOOP ( 'NONE', ( #1729, #16933, #18896, #8452, #15138, #11417 ) ) ;
#27816 = VERTEX_POINT ( 'NONE', #16777 ) ;
#27817 = ORIENTED_EDGE ( 'NONE', *, *, #6805, .T. ) ;
#27818 = DIRECTION ( 'NONE',  ( 0.000000000000000000, 1.000000000000000000, 0.000000000000000000 ) ) ;
#27819 = CARTESIAN_POINT ( 'NONE',  ( 0.4895462770359960136, 0.7878044190915924894, -0.4800777499787165503 ) ) ;
#27820 = DIRECTION ( 'NONE',  ( -1.000000000000000000, 0.000000000000000000, 0.000000000000000000 ) ) ;
#27821 = CARTESIAN_POINT ( 'NONE',  ( -0.4055118110236220486, -0.4724409448818898127, 0.6411263657805708061 ) ) ;
#27822 = EDGE_CURVE ( 'NONE', #11993, #14551, #27866, .T. ) ;
#27823 = AXIS2_PLACEMENT_3D ( 'NONE', #5075, #11582, #20197 ) ;
#27824 = DIRECTION ( 'NONE',  ( 0.000000000000000000, 0.000000000000000000, -1.000000000000000000 ) ) ;
#27825 = VECTOR ( 'NONE', #22654, 39.37007874015748143 ) ;
#27826 = EDGE_CURVE ( 'NONE', #18410, #10367, #18403, .T. ) ;
#27827 = DIRECTION ( 'NONE',  ( 0.000000000000000000, 1.224646799147352221E-16, 1.000000000000000000 ) ) ;
#27828 = AXIS2_PLACEMENT_3D ( 'NONE', #17704, #9217, #2590 ) ;
#27829 = CARTESIAN_POINT ( 'NONE',  ( -0.5646648215863662168, -0.3246897230469174001, 0.1946523111621117075 ) ) ;
#27830 = FACE_BOUND ( 'NONE', #9100, .T. ) ;
#27831 = EDGE_CURVE ( 'NONE', #2655, #27102, #12024, .T. ) ;
#27832 = CARTESIAN_POINT ( 'NONE',  ( -1.928513779527558736E-17, 0.000000000000000000, -0.03543307086614204404 ) ) ;
#27833 = FACE_OUTER_BOUND ( 'NONE', #12652, .T. ) ;
#27834 = DIRECTION ( 'NONE',  ( -1.000000000000000000, 0.000000000000000000, -0.000000000000000000 ) ) ;
#27835 = CARTESIAN_POINT ( 'NONE',  ( -0.09842519684999360974, 0.1968503937007873850, -3.259751644589251818 ) ) ;
#27836 = VERTEX_POINT ( 'NONE', #7639 ) ;
#27837 = EDGE_LOOP ( 'NONE', ( #10844, #6713, #12594, #23847 ) ) ;
#27838 = FACE_OUTER_BOUND ( 'NONE', #15707, .T. ) ;
#27839 = EDGE_CURVE ( 'NONE', #25818, #6360, #3776, .T. ) ;
#27840 = DIRECTION ( 'NONE',  ( 0.000000000000000000, 0.8660254037844385966, 0.4999999999999998335 ) ) ;
#27841 = ADVANCED_FACE ( 'NONE', ( #6741 ), #21848, .F. ) ;
#27842 = ORIENTED_EDGE ( 'NONE', *, *, #14054, .T. ) ;
#27843 = CARTESIAN_POINT ( 'NONE',  ( -0.09842519685039370636, 2.800920866141732248E-17, 0.09092130223458683158 ) ) ;
#27844 = AXIS2_PLACEMENT_3D ( 'NONE', #20913, #22900, #1414 ) ;
#27845 = CARTESIAN_POINT ( 'NONE',  ( -4.821283464566928349E-18, 0.000000000000000000, -0.3779527559055118058 ) ) ;
#27846 = CYLINDRICAL_SURFACE ( 'NONE', #21325, 0.5379714048901780288 ) ;
#27847 = ORIENTED_EDGE ( 'NONE', *, *, #14207, .F. ) ;
#27848 = CARTESIAN_POINT ( 'NONE',  ( 0.3411065095061437402, 0.06065137456822566192, 0.1377952755905510474 ) ) ;
#27849 = ORIENTED_EDGE ( 'NONE', *, *, #23131, .F. ) ;
#27850 = LINE ( 'NONE', #27317, #6633 ) ;
#27851 = CIRCLE ( 'NONE', #19265, 0.2362204724225640262 ) ;
#27852 = CARTESIAN_POINT ( 'NONE',  ( 0.09842519685039355370, 0.2165354330708661457, -3.548228346456693050 ) ) ;
#27853 = STYLED_ITEM ( 'NONE', ( #26915 ), #21926 ) ;
#27854 = DIRECTION ( 'NONE',  ( 0.000000000000000000, 0.000000000000000000, 1.000000000000000000 ) ) ;
#27855 = DIRECTION ( 'NONE',  ( 1.000000000000000000, 0.000000000000000000, 0.000000000000000000 ) ) ;
#27856 = CARTESIAN_POINT ( 'NONE',  ( 0.000000000000000000, 0.000000000000000000, -2.322834645648386154 ) ) ;
#27857 = EDGE_CURVE ( 'NONE', #26290, #12497, #27397, .T. ) ;
#27858 = VERTEX_POINT ( 'NONE', #10831 ) ;
#27859 = CARTESIAN_POINT ( 'NONE',  ( 0.6708219662590964028, -0.1536294932067025498, 0.1322818203437344520 ) ) ;
#27860 = DIRECTION ( 'NONE',  ( -1.000000000000000000, 0.000000000000000000, 0.000000000000000000 ) ) ;
#27861 = DIRECTION ( 'NONE',  ( 1.000000000000000000, 0.000000000000000000, 0.000000000000000000 ) ) ;
#27862 = DIRECTION ( 'NONE',  ( -0.000000000000000000, 1.000000000000000000, -0.000000000000000000 ) ) ;
#27863 = EDGE_CURVE ( 'NONE', #9720, #23369, #13852, .T. ) ;
#27864 = CARTESIAN_POINT ( 'NONE',  ( 0.0005710523241086142487, 0.4632828964888820455, 0.2048502514553257048 ) ) ;
#27865 = CARTESIAN_POINT ( 'NONE',  ( -0.03607471876262473287, 0.5511811023622048555, 0.9399606299212598381 ) ) ;
#27866 = CIRCLE ( 'NONE', #24232, 0.5511811023975373702 ) ;
#27867 = AXIS2_PLACEMENT_3D ( 'NONE', #20583, #18728, #10246 ) ;
#27868 = CARTESIAN_POINT ( 'NONE',  ( -0.5177165354330708347, -0.4724409448818898127, -0.9954570744419902750 ) ) ;
#27870 = CARTESIAN_POINT ( 'NONE',  ( -0.2181198385716950350, 0.2842139414039993039, -3.115157480314961091 ) ) ;
#27871 = AXIS2_PLACEMENT_3D ( 'NONE', #13057, #25916, #8814 ) ;
#27872 = ADVANCED_FACE ( 'NONE', ( #8575 ), #17032, .T. ) ;
#27873 = EDGE_CURVE ( 'NONE', #23663, #9597, #19723, .T. ) ;
#27874 = VERTEX_POINT ( 'NONE', #15059 ) ;
#27875 = ORIENTED_EDGE ( 'NONE', *, *, #22850, .T. ) ;
#27876 = CARTESIAN_POINT ( 'NONE',  ( 0.5085118447796559416, -0.06699507805604926203, -1.550196850393700920 ) ) ;
#27877 = CARTESIAN_POINT ( 'NONE',  ( 0.03746919241598507117, -0.5708675606921427281, 0.9399606299212600602 ) ) ;
#27878 = CARTESIAN_POINT ( 'NONE',  ( -0.4858607088160732390, -0.2805118110236220486, 0.2775610236220472093 ) ) ;
#27879 = DIRECTION ( 'NONE',  ( -0.7071067818211432821, 8.659560570126489743E-17, 0.7071067805519516414 ) ) ;
#27880 = CARTESIAN_POINT ( 'NONE',  ( 0.7874015748031496509, -7.558374153346456878E-06, -2.105236220445303008 ) ) ;
#27881 = VERTEX_POINT ( 'NONE', #9750 ) ;
#27882 = CARTESIAN_POINT ( 'NONE',  ( 0.0005789221761214173069, 0.4692909815006417462, 0.07637795275590551769 ) ) ;
#27883 = NEXT_ASSEMBLY_USAGE_OCCURRENCE ( 'Index Plate:1', ' ', ' ', #7589, #6545, $ ) ;
#27884 = NEXT_ASSEMBLY_USAGE_OCCURRENCE ( 'Output Shaft:1', ' ', ' ', #7589, #6896, $ ) ;
#27885 = NEXT_ASSEMBLY_USAGE_OCCURRENCE ( 'Cam Shaft:1', ' ', ' ', #7589, #18243, $ ) ;
#27886 = NEXT_ASSEMBLY_USAGE_OCCURRENCE ( 'Barrel Cam:1', ' ', ' ', #7589, #19482, $ ) ;
#27887 = NEXT_ASSEMBLY_USAGE_OCCURRENCE ( 'Deep Groove Ball Bearing 15x28x7:1', ' ', ' ', #7589, #16541, $ ) ;
#27888 = NEXT_ASSEMBLY_USAGE_OCCURRENCE ( 'Shaft Seal 15x26x7:1', ' ', ' ', #7589, #669, $ ) ;
#27889 = NEXT_ASSEMBLY_USAGE_OCCURRENCE ( 'Deep Groove Ball Bearing 20x37x9:1', ' ', ' ', #7589, #10324, $ ) ;
#27890 = NEXT_ASSEMBLY_USAGE_OCCURRENCE ( 'Shaft Seal 20x35x7:1', ' ', ' ', #7589, #23987, $ ) ;
#27891 = NEXT_ASSEMBLY_USAGE_OCCURRENCE ( 'Front Bearing Cover:1', ' ', ' ', #7589, #24464, $ ) ;
#27892 = NEXT_ASSEMBLY_USAGE_OCCURRENCE ( 'Rear Bearing Cover:1', ' ', ' ', #7589, #1882, $ ) ;
#27893 = NEXT_ASSEMBLY_USAGE_OCCURRENCE ( 'O-Ring 36.5x2.65:1', ' ', ' ', #7589, #1533, $ ) ;
#27894 = NEXT_ASSEMBLY_USAGE_OCCURRENCE ( 'O-Ring 26.5x2.65:1', ' ', ' ', #7589, #2566, $ ) ;
#27895 = NEXT_ASSEMBLY_USAGE_OCCURRENCE ( 'Cam Follower:1', ' ', ' ', #7589, #26544, $ ) ;
#27896 = NEXT_ASSEMBLY_USAGE_OCCURRENCE ( 'Cam Follower:2', ' ', ' ', #7589, #26544, $ ) ;
#27897 = NEXT_ASSEMBLY_USAGE_OCCURRENCE ( 'Cam Follower:3', ' ', ' ', #7589, #26544, $ ) ;
#27898 = NEXT_ASSEMBLY_USAGE_OCCURRENCE ( 'Cam Follower:4', ' ', ' ', #7589, #26544, $ ) ;
#27899 = NEXT_ASSEMBLY_USAGE_OCCURRENCE ( 'Cam Follower:5', ' ', ' ', #7589, #26544, $ ) ;
#27900 = NEXT_ASSEMBLY_USAGE_OCCURRENCE ( 'Cam Follower:6', ' ', ' ', #7589, #26544, $ ) ;
#27901 = NEXT_ASSEMBLY_USAGE_OCCURRENCE ( 'Cam Follower:7', ' ', ' ', #7589, #26544, $ ) ;
#27902 = NEXT_ASSEMBLY_USAGE_OCCURRENCE ( 'Cam Follower:8', ' ', ' ', #7589, #26544, $ ) ;
#27903 = NEXT_ASSEMBLY_USAGE_OCCURRENCE ( 'M6 Thin Hex Nut:1', ' ', ' ', #7589, #11889, $ ) ;
#27904 = NEXT_ASSEMBLY_USAGE_OCCURRENCE ( 'M6 Thin Hex Nut:2', ' ', ' ', #7589, #11889, $ ) ;
#27905 = NEXT_ASSEMBLY_USAGE_OCCURRENCE ( 'M6 Thin Hex Nut:3', ' ', ' ', #7589, #11889, $ ) ;
#27906 = NEXT_ASSEMBLY_USAGE_OCCURRENCE ( 'M6 Thin Hex Nut:4', ' ', ' ', #7589, #11889, $ ) ;
#27907 = NEXT_ASSEMBLY_USAGE_OCCURRENCE ( 'M6 Thin Hex Nut:5', ' ', ' ', #7589, #11889, $ ) ;
#27908 = NEXT_ASSEMBLY_USAGE_OCCURRENCE ( 'M6 Thin Hex Nut:6', ' ', ' ', #7589, #11889, $ ) ;
#27909 = NEXT_ASSEMBLY_USAGE_OCCURRENCE ( 'M6 Thin Hex Nut:7', ' ', ' ', #7589, #11889, $ ) ;
#27910 = NEXT_ASSEMBLY_USAGE_OCCURRENCE ( 'M6 Thin Hex Nut:8', ' ', ' ', #7589, #11889, $ ) ;
#27911 = NEXT_ASSEMBLY_USAGE_OCCURRENCE ( 'M6 Thin Hex Nut:9', ' ', ' ', #7589, #11889, $ ) ;
#27912 = NEXT_ASSEMBLY_USAGE_OCCURRENCE ( 'M6 Thin Hex Nut:10', ' ', ' ', #7589, #11889, $ ) ;
#27913 = NEXT_ASSEMBLY_USAGE_OCCURRENCE ( 'M6 Thin Hex Nut:11', ' ', ' ', #7589, #11889, $ ) ;
#27914 = NEXT_ASSEMBLY_USAGE_OCCURRENCE ( 'M6 Thin Hex Nut:12', ' ', ' ', #7589, #11889, $ ) ;
#27915 = NEXT_ASSEMBLY_USAGE_OCCURRENCE ( 'M6 Thin Hex Nut:13', ' ', ' ', #7589, #11889, $ ) ;
#27916 = NEXT_ASSEMBLY_USAGE_OCCURRENCE ( 'M6 Thin Hex Nut:14', ' ', ' ', #7589, #11889, $ ) ;
#27917 = NEXT_ASSEMBLY_USAGE_OCCURRENCE ( 'M6 Thin Hex Nut:15', ' ', ' ', #7589, #11889, $ ) ;
#27918 = NEXT_ASSEMBLY_USAGE_OCCURRENCE ( 'M6 Thin Hex Nut:16', ' ', ' ', #7589, #11889, $ ) ;
#27919 = NEXT_ASSEMBLY_USAGE_OCCURRENCE ( 'Deep Groove Ball Bearing 20x42x12:1', ' ', ' ', #7589, #17410, $ ) ;
#27920 = NEXT_ASSEMBLY_USAGE_OCCURRENCE ( 'Tapered Roller Bearing 17x40x17:1', ' ', ' ', #7589, #22417, $ ) ;
#27921 = NEXT_ASSEMBLY_USAGE_OCCURRENCE ( 'ISO 4762 M5x16 Socket Head Cap Screw:1', ' ', ' ', #7589, #2378, $ ) ;
#27922 = NEXT_ASSEMBLY_USAGE_OCCURRENCE ( 'ISO 4762 M5x16 Socket Head Cap Screw:2', ' ', ' ', #7589, #2378, $ ) ;
#27923 = NEXT_ASSEMBLY_USAGE_OCCURRENCE ( 'ISO 4762 M5x16 Socket Head Cap Screw:3', ' ', ' ', #7589, #2378, $ ) ;
#27927 = CARTESIAN_POINT ( '', ( 0.0, 0.0, 0.0 ) ) ;
#27928 = DIRECTION ( '', ( 0.0, 0.0, 1.0 ) ) ;
#27929 = DIRECTION ( '', ( 1.0, 0.0, 0.0 ) ) ;
#27930 = AXIS2_PLACEMENT_3D ( '', #27927, #27928, #27929 ) ;
#27931 = ADVANCED_BREP_SHAPE_REPRESENTATION ( 'Bearing Cup', ( #12201, #27930, #27941 ), #3496 ) ;
#27932 = PRODUCT ( 'Bearing Cup', 'Bearing Cup', '', ( #7554 ) ) ;
#27933 = PRODUCT_DEFINITION_FORMATION_WITH_SPECIFIED_SOURCE ( 'ANY', '', #27932, .NOT_KNOWN. ) ;
#27934 = PRODUCT_DEFINITION ( 'Bearing Cup', '', #27933, #20403 ) ;
#27935 = PRODUCT_DEFINITION_SHAPE ( '', '', #27934 ) ;
#27936 = SHAPE_DEFINITION_REPRESENTATION ( #27935, #27931 ) ;
#27937 = PRODUCT_RELATED_PRODUCT_CATEGORY ( 'part', '', ( #27932 ) ) ;
#27938 = CARTESIAN_POINT ( '', ( 0.0, 0.0, 0.0 ) ) ;
#27939 = DIRECTION ( '', ( 0.0, 0.0, 1.0 ) ) ;
#27940 = DIRECTION ( '', ( 1.0, 0.0, 0.0 ) ) ;
#27941 = AXIS2_PLACEMENT_3D ( '', #27938, #27939, #27940 ) ;
#27942 = CARTESIAN_POINT ( '', ( 0.0, 0.0, 0.0 ) ) ;
#27943 = DIRECTION ( '', ( 0.0, 0.0, 1.0 ) ) ;
#27944 = DIRECTION ( '', ( 1.0, 0.0, 0.0 ) ) ;
#27945 = AXIS2_PLACEMENT_3D ( '', #27942, #27943, #27944 ) ;
#27946 = NEXT_ASSEMBLY_USAGE_OCCURRENCE ( 'Bearing Cup:1', ' ', ' ', #22417, #27934, $ ) ;
#27947 = PRODUCT_DEFINITION_SHAPE ( '', '', #27946 ) ;
#27948 = ITEM_DEFINED_TRANSFORMATION ( '', '', #27945, #27941 ) ;
#27949 = ( REPRESENTATION_RELATIONSHIP ( '', '', #22737, #27931 ) REPRESENTATION_RELATIONSHIP_WITH_TRANSFORMATION ( #27948 ) SHAPE_REPRESENTATION_RELATIONSHIP ( ) ) ;
#27950 = CONTEXT_DEPENDENT_SHAPE_REPRESENTATION ( #27949, #27947 ) ;
#27951 = CARTESIAN_POINT ( '', ( 0.0, 0.0, 0.0 ) ) ;
#27952 = DIRECTION ( '', ( 0.0, 0.0, 1.0 ) ) ;
#27953 = DIRECTION ( '', ( 1.0, 0.0, 0.0 ) ) ;
#27954 = AXIS2_PLACEMENT_3D ( '', #27951, #27952, #27953 ) ;
#27955 = ADVANCED_BREP_SHAPE_REPRESENTATION ( 'Bearing Cone', ( #21416, #27954, #27965 ), #3496 ) ;
#27956 = PRODUCT ( 'Bearing Cone', 'Bearing Cone', '', ( #7554 ) ) ;
#27957 = PRODUCT_DEFINITION_FORMATION_WITH_SPECIFIED_SOURCE ( 'ANY', '', #27956, .NOT_KNOWN. ) ;
#27958 = PRODUCT_DEFINITION ( 'Bearing Cone', '', #27957, #20403 ) ;
#27959 = PRODUCT_DEFINITION_SHAPE ( '', '', #27958 ) ;
#27960 = SHAPE_DEFINITION_REPRESENTATION ( #27959, #27955 ) ;
#27961 = PRODUCT_RELATED_PRODUCT_CATEGORY ( 'part', '', ( #27956 ) ) ;
#27962 = CARTESIAN_POINT ( '', ( 0.0, 0.0, 0.0 ) ) ;
#27963 = DIRECTION ( '', ( 0.0, 0.0, 1.0 ) ) ;
#27964 = DIRECTION ( '', ( 1.0, 0.0, 0.0 ) ) ;
#27965 = AXIS2_PLACEMENT_3D ( '', #27962, #27963, #27964 ) ;
#27966 = CARTESIAN_POINT ( '', ( 0.0, 0.0, 0.0 ) ) ;
#27967 = DIRECTION ( '', ( 0.0, 0.0, 1.0 ) ) ;
#27968 = DIRECTION ( '', ( 1.0, 0.0, 0.0 ) ) ;
#27969 = AXIS2_PLACEMENT_3D ( '', #27966, #27967, #27968 ) ;
#27970 = NEXT_ASSEMBLY_USAGE_OCCURRENCE ( 'Bearing Cone:1', ' ', ' ', #22417, #27958, $ ) ;
#27971 = PRODUCT_DEFINITION_SHAPE ( '', '', #27970 ) ;
#27972 = ITEM_DEFINED_TRANSFORMATION ( '', '', #27969, #27965 ) ;
#27973 = ( REPRESENTATION_RELATIONSHIP ( '', '', #22737, #27955 ) REPRESENTATION_RELATIONSHIP_WITH_TRANSFORMATION ( #27972 ) SHAPE_REPRESENTATION_RELATIONSHIP ( ) ) ;
#27974 = CONTEXT_DEPENDENT_SHAPE_REPRESENTATION ( #27973, #27971 ) ;
#27975 = CARTESIAN_POINT ( '', ( 0.0, 0.0, 0.0 ) ) ;
#27976 = DIRECTION ( '', ( 0.0, 0.0, 1.0 ) ) ;
#27977 = DIRECTION ( '', ( 1.0, 0.0, 0.0 ) ) ;
#27978 = AXIS2_PLACEMENT_3D ( '', #27975, #27976, #27977 ) ;
#27979 = CARTESIAN_POINT ( '', ( 1.8025436886152346, 2.925196850393701, 0.7677165354330673 ) ) ;
#27980 = DIRECTION ( '', ( 1.2958717723672432e-06, -1.138024988063455e-14, -0.9999999999991604 ) ) ;
#27981 = DIRECTION ( '', ( 6.465977648611864e-15, -1.0, 1.143642754752177e-14 ) ) ;
#27982 = AXIS2_PLACEMENT_3D ( '', #27979, #27980, #27981 ) ;
#27983 = NEXT_ASSEMBLY_USAGE_OCCURRENCE ( 'ISO 4762 M5x16 Socket Head Cap Screw:4', ' ', ' ', #7589, #2378, $ ) ;
#27984 = PRODUCT_DEFINITION_SHAPE ( '', '', #27983 ) ;
#27985 = ITEM_DEFINED_TRANSFORMATION ( '', '', #27982, #27978 ) ;
#27986 = ( REPRESENTATION_RELATIONSHIP ( '', '', #12434, #9188 ) REPRESENTATION_RELATIONSHIP_WITH_TRANSFORMATION ( #27985 ) SHAPE_REPRESENTATION_RELATIONSHIP ( ) ) ;
#27987 = CONTEXT_DEPENDENT_SHAPE_REPRESENTATION ( #27986, #27984 ) ;
#27988 = CARTESIAN_POINT ( '', ( 0.0, 0.0, 0.0 ) ) ;
#27989 = DIRECTION ( '', ( 0.0, 0.0, 1.0 ) ) ;
#27990 = DIRECTION ( '', ( 1.0, 0.0, 0.0 ) ) ;
#27991 = AXIS2_PLACEMENT_3D ( '', #27988, #27989, #27990 ) ;
#27992 = CARTESIAN_POINT ( '', ( 0.9842519685039354, 2.925196850393701, -0.6496062992126019 ) ) ;
#27993 = DIRECTION ( '', ( 1.2958717723672432e-06, -1.138024988063455e-14, -0.9999999999991604 ) ) ;
#27994 = DIRECTION ( '', ( 6.465977648611864e-15, -1.0, 1.143642754752177e-14 ) ) ;
#27995 = AXIS2_PLACEMENT_3D ( '', #27992, #27993, #27994 ) ;
#27996 = NEXT_ASSEMBLY_USAGE_OCCURRENCE ( 'ISO 4762 M5x16 Socket Head Cap Screw:5', ' ', ' ', #7589, #2378, $ ) ;
#27997 = PRODUCT_DEFINITION_SHAPE ( '', '', #27996 ) ;
#27998 = ITEM_DEFINED_TRANSFORMATION ( '', '', #27995, #27991 ) ;
#27999 = ( REPRESENTATION_RELATIONSHIP ( '', '', #12434, #9188 ) REPRESENTATION_RELATIONSHIP_WITH_TRANSFORMATION ( #27998 ) SHAPE_REPRESENTATION_RELATIONSHIP ( ) ) ;
#28000 = CONTEXT_DEPENDENT_SHAPE_REPRESENTATION ( #27999, #27997 ) ;
#28001 = CARTESIAN_POINT ( '', ( 0.0, 0.0, 0.0 ) ) ;
#28002 = DIRECTION ( '', ( 0.0, 0.0, 1.0 ) ) ;
#28003 = DIRECTION ( '', ( 1.0, 0.0, 0.0 ) ) ;
#28004 = AXIS2_PLACEMENT_3D ( '', #28001, #28002, #28003 ) ;
#28005 = CARTESIAN_POINT ( '', ( 0.1659602483926361, 2.925196850393701, 0.7677165354330673 ) ) ;
#28006 = DIRECTION ( '', ( 1.2958717723672432e-06, -1.138024988063455e-14, -0.9999999999991604 ) ) ;
#28007 = DIRECTION ( '', ( 6.465977648611864e-15, -1.0, 1.143642754752177e-14 ) ) ;
#28008 = AXIS2_PLACEMENT_3D ( '', #28005, #28006, #28007 ) ;
#28009 = NEXT_ASSEMBLY_USAGE_OCCURRENCE ( 'ISO 4762 M5x16 Socket Head Cap Screw:6', ' ', ' ', #7589, #2378, $ ) ;
#28010 = PRODUCT_DEFINITION_SHAPE ( '', '', #28009 ) ;
#28011 = ITEM_DEFINED_TRANSFORMATION ( '', '', #28008, #28004 ) ;
#28012 = ( REPRESENTATION_RELATIONSHIP ( '', '', #12434, #9188 ) REPRESENTATION_RELATIONSHIP_WITH_TRANSFORMATION ( #28011 ) SHAPE_REPRESENTATION_RELATIONSHIP ( ) ) ;
#28013 = CONTEXT_DEPENDENT_SHAPE_REPRESENTATION ( #28012, #28010 ) ;
ENDSEC;
END-ISO-10303-21;
